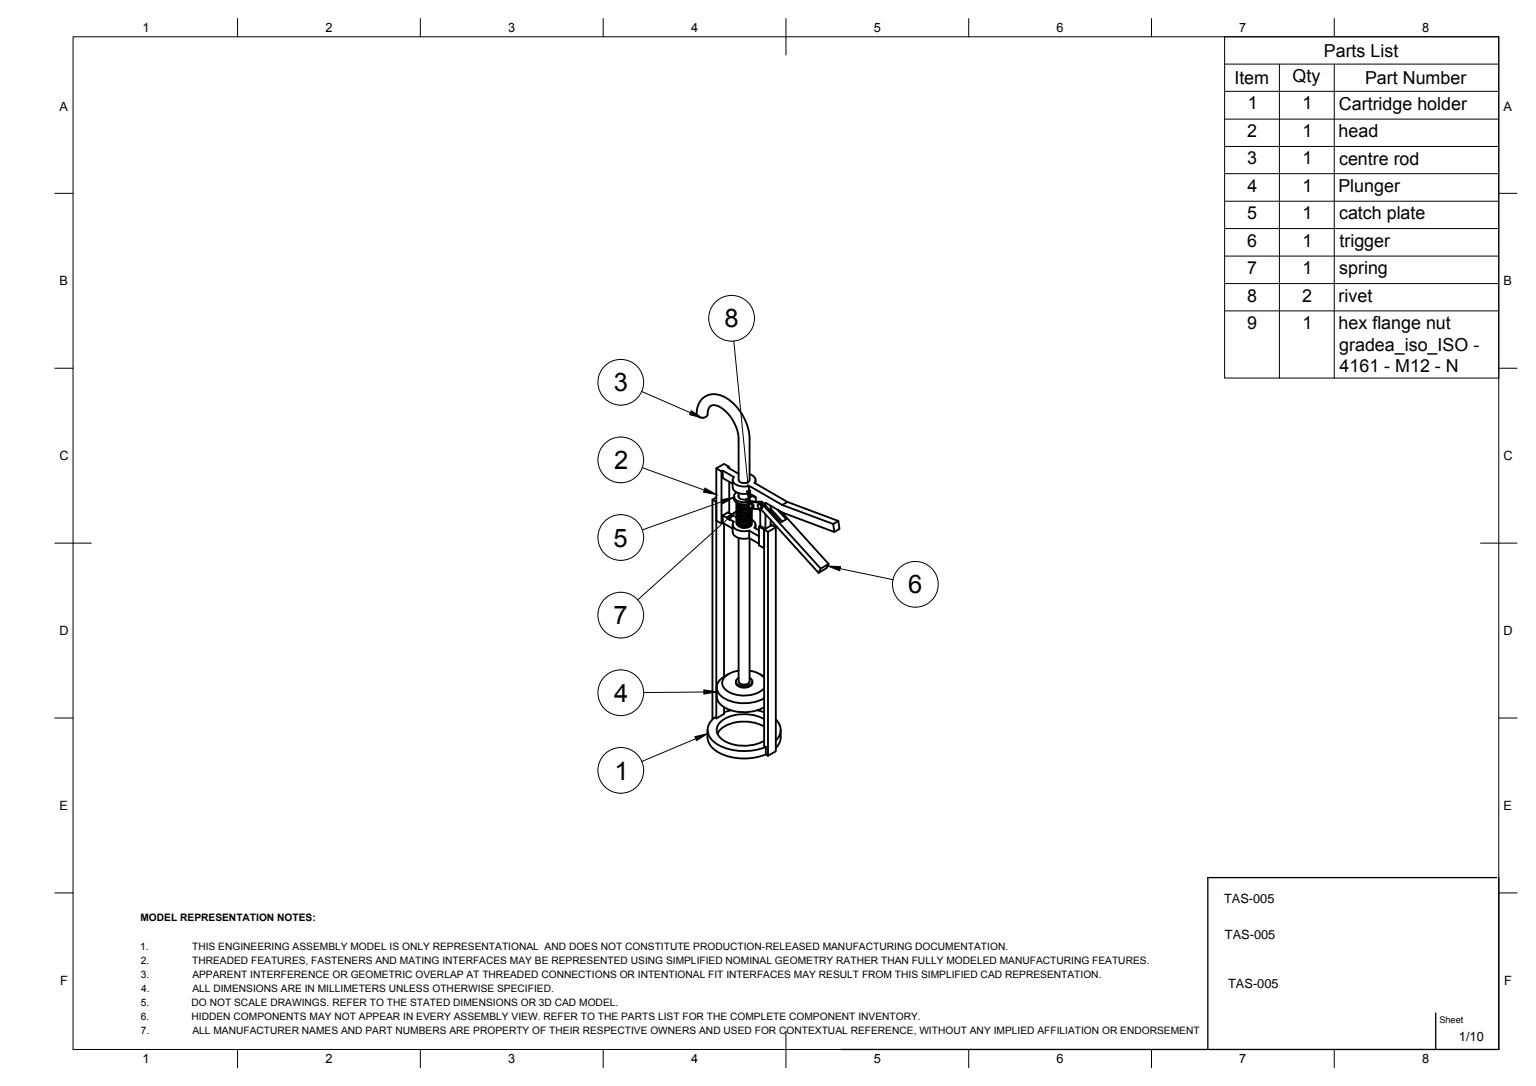
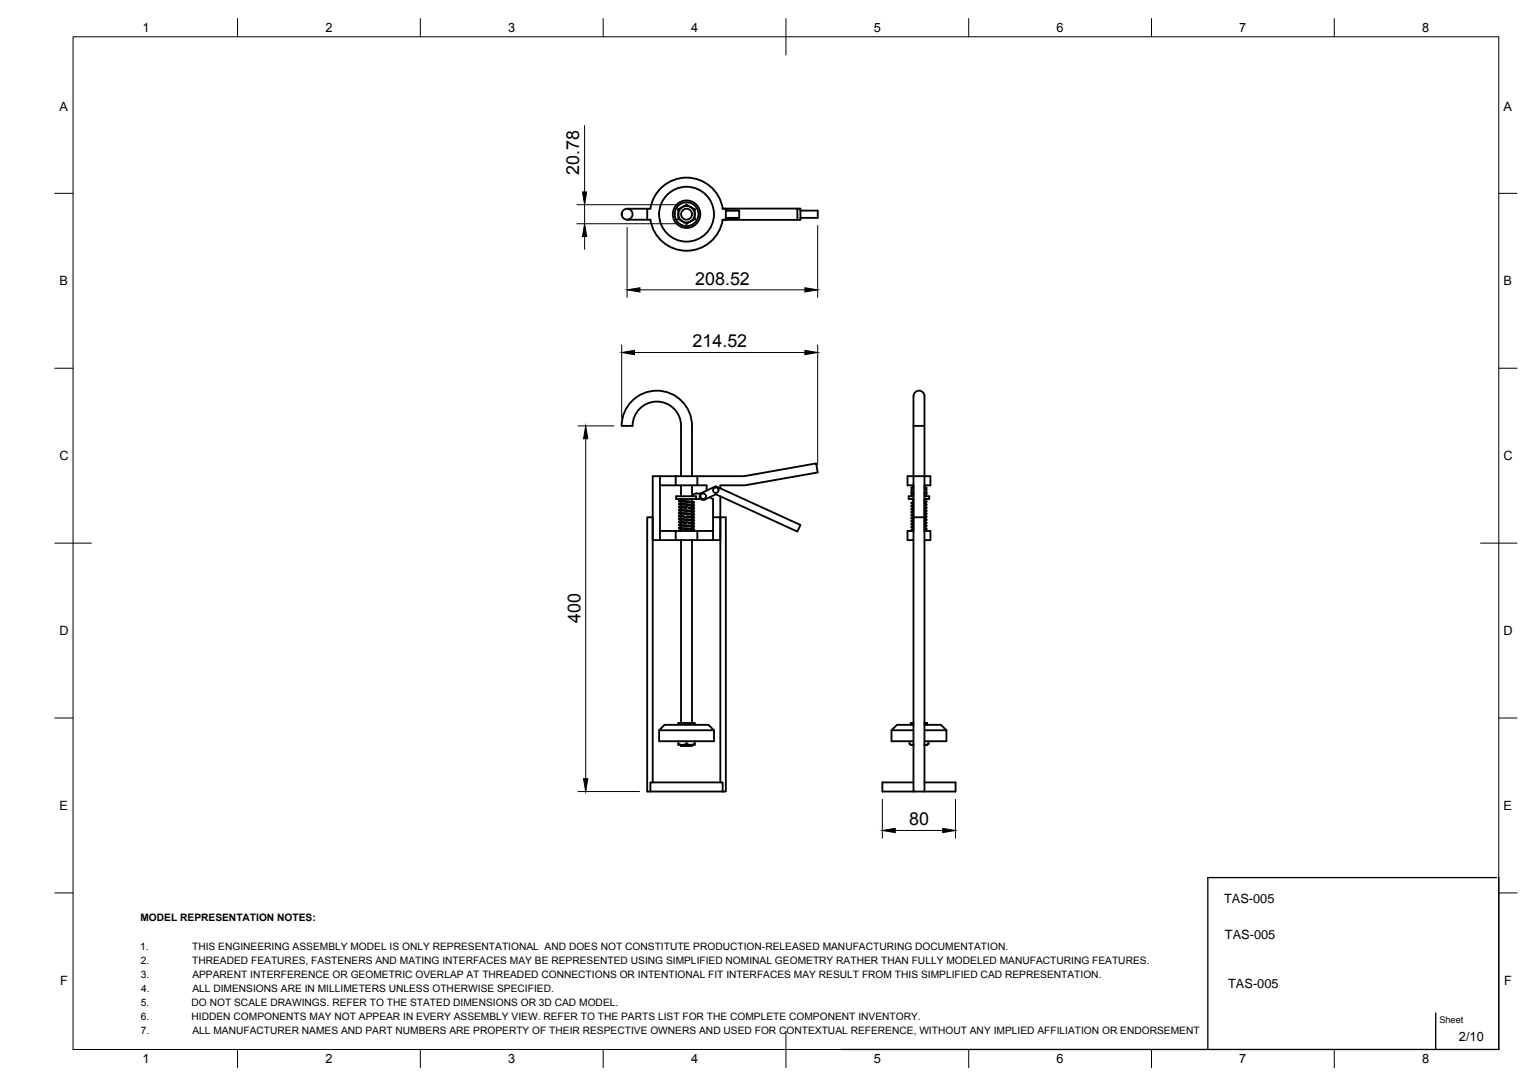
ISO-10303-21;
HEADER;
/* Generated by software containing ST-Developer
 * from STEP Tools, Inc. (www.steptools.com) 
 */

FILE_DESCRIPTION(
/* description */ ('STEP AP214'),
/* implementation_level */ '2;1');

FILE_NAME(
/* name */ 'TAS-005',
/* time_stamp */ '2026-11-04T19:54:22-08:00',
/* author */ (''),
/* organization */ (''),
/* preprocessor_version */ 'ST-DEVELOPER v20.2',
/* originating_system */ 'Autodesk Translation Framework v15.17.0.0',
/* authorisation */ '');

FILE_SCHEMA (('AUTOMOTIVE_DESIGN { 1 0 10303 214 3 1 1 }'));
ENDSEC;

DATA;
#10=MECHANICAL_DESIGN_GEOMETRIC_PRESENTATION_REPRESENTATION('',(#239,#240,
#241,#242,#243,#244,#245,#246,#247),#14084);
#11=ITEM_DEFINED_TRANSFORMATION($,$,#3575,#3854);
#12=ITEM_DEFINED_TRANSFORMATION($,$,#3597,#3855);
#13=ITEM_DEFINED_TRANSFORMATION($,$,#3649,#3856);
#14=ITEM_DEFINED_TRANSFORMATION($,$,#3725,#3857);
#15=ITEM_DEFINED_TRANSFORMATION($,$,#3741,#3858);
#16=ITEM_DEFINED_TRANSFORMATION($,$,#3763,#3859);
#17=ITEM_DEFINED_TRANSFORMATION($,$,#3794,#3860);
#18=ITEM_DEFINED_TRANSFORMATION($,$,#3840,#3861);
#19=ITEM_DEFINED_TRANSFORMATION($,$,#3802,#3862);
#20=ITEM_DEFINED_TRANSFORMATION($,$,#3840,#3863);
#21=(
REPRESENTATION_RELATIONSHIP($,$,#14120,#14119)
REPRESENTATION_RELATIONSHIP_WITH_TRANSFORMATION(#11)
SHAPE_REPRESENTATION_RELATIONSHIP()
);
#22=(
REPRESENTATION_RELATIONSHIP($,$,#14121,#14119)
REPRESENTATION_RELATIONSHIP_WITH_TRANSFORMATION(#12)
SHAPE_REPRESENTATION_RELATIONSHIP()
);
#23=(
REPRESENTATION_RELATIONSHIP($,$,#14122,#14119)
REPRESENTATION_RELATIONSHIP_WITH_TRANSFORMATION(#13)
SHAPE_REPRESENTATION_RELATIONSHIP()
);
#24=(
REPRESENTATION_RELATIONSHIP($,$,#14123,#14119)
REPRESENTATION_RELATIONSHIP_WITH_TRANSFORMATION(#14)
SHAPE_REPRESENTATION_RELATIONSHIP()
);
#25=(
REPRESENTATION_RELATIONSHIP($,$,#14124,#14119)
REPRESENTATION_RELATIONSHIP_WITH_TRANSFORMATION(#15)
SHAPE_REPRESENTATION_RELATIONSHIP()
);
#26=(
REPRESENTATION_RELATIONSHIP($,$,#14125,#14119)
REPRESENTATION_RELATIONSHIP_WITH_TRANSFORMATION(#16)
SHAPE_REPRESENTATION_RELATIONSHIP()
);
#27=(
REPRESENTATION_RELATIONSHIP($,$,#14126,#14119)
REPRESENTATION_RELATIONSHIP_WITH_TRANSFORMATION(#17)
SHAPE_REPRESENTATION_RELATIONSHIP()
);
#28=(
REPRESENTATION_RELATIONSHIP($,$,#14128,#14119)
REPRESENTATION_RELATIONSHIP_WITH_TRANSFORMATION(#18)
SHAPE_REPRESENTATION_RELATIONSHIP()
);
#29=(
REPRESENTATION_RELATIONSHIP($,$,#14127,#14119)
REPRESENTATION_RELATIONSHIP_WITH_TRANSFORMATION(#19)
SHAPE_REPRESENTATION_RELATIONSHIP()
);
#30=(
REPRESENTATION_RELATIONSHIP($,$,#14128,#14119)
REPRESENTATION_RELATIONSHIP_WITH_TRANSFORMATION(#20)
SHAPE_REPRESENTATION_RELATIONSHIP()
);
#31=CONTEXT_DEPENDENT_SHAPE_REPRESENTATION(#21,#14109);
#32=CONTEXT_DEPENDENT_SHAPE_REPRESENTATION(#22,#14110);
#33=CONTEXT_DEPENDENT_SHAPE_REPRESENTATION(#23,#14111);
#34=CONTEXT_DEPENDENT_SHAPE_REPRESENTATION(#24,#14112);
#35=CONTEXT_DEPENDENT_SHAPE_REPRESENTATION(#25,#14113);
#36=CONTEXT_DEPENDENT_SHAPE_REPRESENTATION(#26,#14114);
#37=CONTEXT_DEPENDENT_SHAPE_REPRESENTATION(#27,#14115);
#38=CONTEXT_DEPENDENT_SHAPE_REPRESENTATION(#28,#14116);
#39=CONTEXT_DEPENDENT_SHAPE_REPRESENTATION(#29,#14117);
#40=CONTEXT_DEPENDENT_SHAPE_REPRESENTATION(#30,#14118);
#41=NEXT_ASSEMBLY_USAGE_OCCURRENCE('Cartridge holder:1',
'Cartridge holder:1','Cartridge holder:1',#14130,#14131,
'Cartridge holder:1');
#42=NEXT_ASSEMBLY_USAGE_OCCURRENCE('head:1','head:1','head:1',#14130,#14132,
'head:1');
#43=NEXT_ASSEMBLY_USAGE_OCCURRENCE('centre rod:1','centre rod:1',
'centre rod:1',#14130,#14133,'centre rod:1');
#44=NEXT_ASSEMBLY_USAGE_OCCURRENCE('plunger:1','plunger:1','plunger:1',
#14130,#14134,'plunger:1');
#45=NEXT_ASSEMBLY_USAGE_OCCURRENCE('catch plate:1','catch plate:1',
'catch plate:1',#14130,#14135,'catch plate:1');
#46=NEXT_ASSEMBLY_USAGE_OCCURRENCE('trigger:1','trigger:1','trigger:1',
#14130,#14136,'trigger:1');
#47=NEXT_ASSEMBLY_USAGE_OCCURRENCE('spring:1','spring:1','spring:1',#14130,
#14137,'spring:1');
#48=NEXT_ASSEMBLY_USAGE_OCCURRENCE('rivet:1','rivet:1','rivet:1',#14130,
#14139,'rivet:1');
#49=NEXT_ASSEMBLY_USAGE_OCCURRENCE(
'hex flange nut gradea_iso_ISO - 4161 - M12 - N:1',
'hex flange nut gradea_iso_ISO - 4161 - M12 - N:1',
'hex flange nut gradea_iso_ISO - 4161 - M12 - N:1',#14130,#14138,
'hex flange nut gradea_iso_ISO - 4161 - M12 - N:1');
#50=NEXT_ASSEMBLY_USAGE_OCCURRENCE('rivet:2','rivet:2','rivet:2',#14130,
#14139,'rivet:2');
#51=CONICAL_SURFACE('',#3729,30.,0.78539816339745);
#52=CONICAL_SURFACE('',#3807,6.,0.959931088596879);
#53=CONICAL_SURFACE('',#3810,5.01,0.959931088596881);
#54=CONICAL_SURFACE('',#3813,12.389406481562,1.22173047639605);
#55=CONICAL_SURFACE('',#3834,9.,0.85944549144248);
#56=CONICAL_SURFACE('',#3835,9.,0.85944549144248);
#57=CONICAL_SURFACE('',#3836,9.,0.85944549144248);
#58=CONICAL_SURFACE('',#3837,9.,0.85944549144248);
#59=CONICAL_SURFACE('',#3838,9.,0.85944549144248);
#60=CONICAL_SURFACE('',#3839,9.,0.85944549144248);
#61=(
BOUNDED_SURFACE()
B_SPLINE_SURFACE(1,2,((#7888,#7889,#7890,#7891,#7892,#7893,#7894,#7895,
#7896,#7897,#7898,#7899,#7900,#7901,#7902,#7903,#7904,#7905,#7906,#7907,
#7908,#7909,#7910,#7911,#7912,#7913,#7914,#7915,#7916,#7917,#7918,#7919,
#7920,#7921,#7922,#7923,#7924,#7925,#7926,#7927,#7928,#7929,#7930,#7931,
#7932,#7933,#7934,#7935,#7936,#7937,#7938,#7939,#7940,#7941,#7942,#7943,
#7944,#7945,#7946,#7947,#7948,#7949,#7950,#7951,#7952,#7953,#7954,#7955,
#7956,#7957,#7958,#7959,#7960,#7961,#7962,#7963,#7964,#7965,#7966,#7967,
#7968,#7969,#7970,#7971,#7972,#7973,#7974,#7975,#7976,#7977,#7978,#7979,
#7980,#7981,#7982,#7983,#7984,#7985,#7986,#7987,#7988,#7989,#7990,#7991,
#7992,#7993,#7994,#7995,#7996,#7997,#7998,#7999,#8000,#8001,#8002,#8003,
#8004,#8005,#8006,#8007,#8008,#8009,#8010,#8011,#8012,#8013,#8014,#8015,
#8016,#8017,#8018,#8019,#8020,#8021,#8022,#8023,#8024,#8025,#8026,#8027,
#8028,#8029,#8030,#8031,#8032,#8033,#8034,#8035,#8036,#8037,#8038,#8039,
#8040,#8041,#8042,#8043,#8044,#8045,#8046,#8047,#8048,#8049,#8050,#8051,
#8052,#8053,#8054,#8055,#8056,#8057,#8058,#8059,#8060,#8061,#8062,#8063,
#8064,#8065,#8066,#8067,#8068,#8069,#8070,#8071,#8072,#8073,#8074,#8075,
#8076,#8077,#8078,#8079,#8080,#8081,#8082,#8083,#8084,#8085,#8086,#8087,
#8088,#8089,#8090,#8091,#8092,#8093,#8094,#8095,#8096,#8097,#8098,#8099,
#8100,#8101,#8102,#8103,#8104,#8105,#8106,#8107,#8108,#8109,#8110,#8111,
#8112,#8113,#8114,#8115,#8116,#8117,#8118,#8119,#8120,#8121,#8122,#8123,
#8124,#8125,#8126,#8127,#8128,#8129,#8130,#8131,#8132,#8133,#8134,#8135,
#8136,#8137,#8138,#8139,#8140,#8141,#8142,#8143,#8144,#8145,#8146,#8147,
#8148,#8149,#8150,#8151,#8152,#8153,#8154,#8155,#8156,#8157,#8158,#8159,
#8160,#8161,#8162,#8163,#8164,#8165,#8166,#8167,#8168,#8169,#8170,#8171,
#8172,#8173,#8174,#8175,#8176,#8177,#8178,#8179,#8180,#8181,#8182,#8183,
#8184,#8185,#8186,#8187,#8188,#8189,#8190,#8191,#8192,#8193,#8194,#8195,
#8196,#8197,#8198,#8199,#8200,#8201,#8202,#8203,#8204,#8205,#8206,#8207,
#8208),(#8209,#8210,#8211,#8212,#8213,#8214,#8215,#8216,#8217,#8218,#8219,
#8220,#8221,#8222,#8223,#8224,#8225,#8226,#8227,#8228,#8229,#8230,#8231,
#8232,#8233,#8234,#8235,#8236,#8237,#8238,#8239,#8240,#8241,#8242,#8243,
#8244,#8245,#8246,#8247,#8248,#8249,#8250,#8251,#8252,#8253,#8254,#8255,
#8256,#8257,#8258,#8259,#8260,#8261,#8262,#8263,#8264,#8265,#8266,#8267,
#8268,#8269,#8270,#8271,#8272,#8273,#8274,#8275,#8276,#8277,#8278,#8279,
#8280,#8281,#8282,#8283,#8284,#8285,#8286,#8287,#8288,#8289,#8290,#8291,
#8292,#8293,#8294,#8295,#8296,#8297,#8298,#8299,#8300,#8301,#8302,#8303,
#8304,#8305,#8306,#8307,#8308,#8309,#8310,#8311,#8312,#8313,#8314,#8315,
#8316,#8317,#8318,#8319,#8320,#8321,#8322,#8323,#8324,#8325,#8326,#8327,
#8328,#8329,#8330,#8331,#8332,#8333,#8334,#8335,#8336,#8337,#8338,#8339,
#8340,#8341,#8342,#8343,#8344,#8345,#8346,#8347,#8348,#8349,#8350,#8351,
#8352,#8353,#8354,#8355,#8356,#8357,#8358,#8359,#8360,#8361,#8362,#8363,
#8364,#8365,#8366,#8367,#8368,#8369,#8370,#8371,#8372,#8373,#8374,#8375,
#8376,#8377,#8378,#8379,#8380,#8381,#8382,#8383,#8384,#8385,#8386,#8387,
#8388,#8389,#8390,#8391,#8392,#8393,#8394,#8395,#8396,#8397,#8398,#8399,
#8400,#8401,#8402,#8403,#8404,#8405,#8406,#8407,#8408,#8409,#8410,#8411,
#8412,#8413,#8414,#8415,#8416,#8417,#8418,#8419,#8420,#8421,#8422,#8423,
#8424,#8425,#8426,#8427,#8428,#8429,#8430,#8431,#8432,#8433,#8434,#8435,
#8436,#8437,#8438,#8439,#8440,#8441,#8442,#8443,#8444,#8445,#8446,#8447,
#8448,#8449,#8450,#8451,#8452,#8453,#8454,#8455,#8456,#8457,#8458,#8459,
#8460,#8461,#8462,#8463,#8464,#8465,#8466,#8467,#8468,#8469,#8470,#8471,
#8472,#8473,#8474,#8475,#8476,#8477,#8478,#8479,#8480,#8481,#8482,#8483,
#8484,#8485,#8486,#8487,#8488,#8489,#8490,#8491,#8492,#8493,#8494,#8495,
#8496,#8497,#8498,#8499,#8500,#8501,#8502,#8503,#8504,#8505,#8506,#8507,
#8508,#8509,#8510,#8511,#8512,#8513,#8514,#8515,#8516,#8517,#8518,#8519,
#8520,#8521,#8522,#8523,#8524,#8525,#8526,#8527,#8528,#8529)),
 .UNSPECIFIED.,.F.,.F.,.F.)
B_SPLINE_SURFACE_WITH_KNOTS((2,2),(3,2,2,2,2,2,2,2,2,2,2,2,2,2,2,2,2,2,
2,2,2,2,2,2,2,2,2,2,2,2,2,2,2,2,2,2,2,2,2,2,2,2,2,2,2,2,2,2,2,2,2,2,2,2,
2,2,2,2,2,2,2,2,2,2,2,2,2,2,2,2,2,2,2,2,2,2,2,2,2,2,2,2,2,2,2,2,2,2,2,2,
2,2,2,2,2,2,2,2,2,2,2,2,2,2,2,2,2,2,2,2,2,2,2,2,2,2,2,2,2,2,2,2,2,2,2,2,
2,2,2,2,2,2,2,2,2,2,2,2,2,2,2,2,2,2,2,2,2,2,2,2,2,2,2,2,2,2,2,2,2,2,3),
(0.,1.),(0.,0.00617283950617284,0.0123456790123457,0.0185185185185185,0.0246913580246914,
0.0308641975308642,0.037037037037037,0.0432098765432099,0.0493827160493827,
0.0555555555555556,0.0617283950617284,0.0679012345679012,0.0740740740740741,
0.0802469135802469,0.0864197530864197,0.0925925925925926,0.0987654320987654,
0.104938271604938,0.111111111111111,0.117283950617284,0.123456790123457,
0.12962962962963,0.135802469135802,0.141975308641975,0.148148148148148,
0.154320987654321,0.160493827160494,0.166666666666667,0.172839506172839,
0.179012345679012,0.185185185185185,0.191358024691358,0.197530864197531,
0.203703703703704,0.209876543209877,0.216049382716049,0.222222222222222,
0.228395061728395,0.234567901234568,0.240740740740741,0.246913580246914,
0.253086419753086,0.259259259259259,0.265432098765432,0.271604938271605,
0.277777777777778,0.283950617283951,0.290123456790123,0.296296296296296,
0.302469135802469,0.308641975308642,0.314814814814815,0.320987654320988,
0.327160493827161,0.333333333333333,0.339506172839506,0.345679012345679,
0.351851851851852,0.358024691358025,0.364197530864198,0.37037037037037,
0.376543209876543,0.382716049382716,0.388888888888889,0.395061728395062,
0.401234567901235,0.407407407407407,0.41358024691358,0.419753086419753,
0.425925925925926,0.432098765432099,0.438271604938272,0.444444444444444,
0.450617283950617,0.45679012345679,0.462962962962963,0.469135802469136,
0.475308641975309,0.481481481481481,0.487654320987654,0.493827160493827,
0.5,0.506172839506173,0.512345679012346,0.518518518518518,0.524691358024691,
0.530864197530864,0.537037037037037,0.54320987654321,0.549382716049383,
0.555555555555556,0.561728395061728,0.567901234567901,0.574074074074074,
0.580246913580247,0.58641975308642,0.592592592592593,0.598765432098765,
0.604938271604938,0.611111111111111,0.617283950617284,0.623456790123457,
0.62962962962963,0.635802469135803,0.641975308641975,0.648148148148148,
0.654320987654321,0.660493827160494,0.666666666666667,0.672839506172839,
0.679012345679012,0.685185185185185,0.691358024691358,0.697530864197531,
0.703703703703704,0.709876543209877,0.716049382716049,0.722222222222222,
0.728395061728395,0.734567901234568,0.740740740740741,0.746913580246914,
0.753086419753086,0.759259259259259,0.765432098765432,0.771604938271605,
0.777777777777778,0.783950617283951,0.790123456790123,0.796296296296296,
0.802469135802469,0.808641975308642,0.814814814814815,0.820987654320988,
0.827160493827161,0.833333333333333,0.839506172839506,0.845679012345679,
0.851851851851852,0.858024691358025,0.864197530864197,0.87037037037037,
0.876543209876543,0.882716049382716,0.888888888888889,0.895061728395062,
0.901234567901235,0.907407407407407,0.91358024691358,0.919753086419753,
0.925925925925926,0.932098765432099,0.938271604938272,0.944444444444444,
0.950617283950617,0.95679012345679,0.962962962962963,0.969135802469136,
0.975308641975309,0.981481481481482,0.987654320987654),.UNSPECIFIED.)
GEOMETRIC_REPRESENTATION_ITEM()
RATIONAL_B_SPLINE_SURFACE(((1.,0.866025403784439,1.,0.866025403784439,1.,
0.866025403784439,1.,0.866025403784439,1.,0.866025403784439,1.,0.866025403784439,
1.,0.866025403784439,1.,0.866025403784439,1.,0.866025403784439,1.,0.866025403784439,
1.,0.866025403784439,1.,0.866025403784439,1.,0.866025403784439,1.,0.866025403784439,
1.,0.866025403784439,1.,0.866025403784439,1.,0.866025403784439,1.,0.866025403784439,
1.,0.866025403784439,1.,0.866025403784439,1.,0.866025403784439,1.,0.866025403784439,
1.,0.866025403784439,1.,0.866025403784439,1.,0.866025403784439,1.,0.866025403784439,
1.,0.866025403784439,1.,0.866025403784439,1.,0.866025403784439,1.,0.866025403784439,
1.,0.866025403784439,1.,0.866025403784439,1.,0.866025403784439,1.,0.866025403784439,
1.,0.866025403784439,1.,0.866025403784439,1.,0.866025403784439,1.,0.866025403784439,
1.,0.866025403784439,1.,0.866025403784439,1.,0.866025403784439,1.,0.866025403784439,
1.,0.866025403784439,1.,0.866025403784439,1.,0.866025403784439,1.,0.866025403784439,
1.,0.866025403784439,1.,0.866025403784439,1.,0.866025403784439,1.,0.866025403784439,
1.,0.866025403784439,1.,0.866025403784439,1.,0.866025403784439,1.,0.866025403784439,
1.,0.866025403784439,1.,0.866025403784439,1.,0.866025403784439,1.,0.866025403784439,
1.,0.866025403784439,1.,0.866025403784439,1.,0.866025403784439,1.,0.866025403784439,
1.,0.866025403784439,1.,0.866025403784439,1.,0.866025403784439,1.,0.866025403784439,
1.,0.866025403784439,1.,0.866025403784439,1.,0.866025403784439,1.,0.866025403784439,
1.,0.866025403784439,1.,0.866025403784439,1.,0.866025403784439,1.,0.866025403784439,
1.,0.866025403784439,1.,0.866025403784439,1.,0.866025403784439,1.,0.866025403784439,
1.,0.866025403784439,1.,0.866025403784439,1.,0.866025403784439,1.,0.866025403784439,
1.,0.866025403784439,1.,0.866025403784439,1.,0.866025403784439,1.,0.866025403784439,
1.,0.866025403784439,1.,0.866025403784439,1.,0.866025403784439,1.,0.866025403784439,
1.,0.866025403784439,1.,0.866025403784439,1.,0.866025403784439,1.,0.866025403784439,
1.,0.866025403784439,1.,0.866025403784439,1.,0.866025403784439,1.,0.866025403784439,
1.,0.866025403784439,1.,0.866025403784439,1.,0.866025403784439,1.,0.866025403784439,
1.,0.866025403784439,1.,0.866025403784439,1.,0.866025403784439,1.,0.866025403784439,
1.,0.866025403784439,1.,0.866025403784439,1.,0.866025403784439,1.,0.866025403784439,
1.,0.866025403784439,1.,0.866025403784439,1.,0.866025403784439,1.,0.866025403784439,
1.,0.866025403784439,1.,0.866025403784439,1.,0.866025403784439,1.,0.866025403784439,
1.,0.866025403784439,1.,0.866025403784439,1.,0.866025403784439,1.,0.866025403784439,
1.,0.866025403784439,1.,0.866025403784439,1.,0.866025403784439,1.,0.866025403784439,
1.,0.866025403784439,1.,0.866025403784439,1.,0.866025403784439,1.,0.866025403784439,
1.,0.866025403784439,1.,0.866025403784439,1.,0.866025403784439,1.,0.866025403784439,
1.,0.866025403784439,1.,0.866025403784439,1.,0.866025403784439,1.,0.866025403784439,
1.,0.866025403784439,1.,0.866025403784439,1.,0.866025403784439,1.,0.866025403784439,
1.,0.866025403784439,1.,0.866025403784439,1.,0.866025403784439,1.,0.866025403784439,
1.,0.866025403784439,1.,0.866025403784439,1.,0.866025403784439,1.,0.866025403784439,
1.,0.866025403784439,1.,0.866025403784439,1.,0.866025403784439,1.,0.866025403784439,
1.,0.866025403784439,1.,0.866025403784439,1.,0.866025403784439,1.,0.866025403784439,
1.,0.866025403784439,1.,0.866025403784439,1.),(1.,0.866025403784439,1.,
0.866025403784439,1.,0.866025403784439,1.,0.866025403784439,1.,0.866025403784439,
1.,0.866025403784439,1.,0.866025403784439,1.,0.866025403784439,1.,0.866025403784439,
1.,0.866025403784439,1.,0.866025403784439,1.,0.866025403784439,1.,0.866025403784439,
1.,0.866025403784439,1.,0.866025403784439,1.,0.866025403784439,1.,0.866025403784439,
1.,0.866025403784439,1.,0.866025403784439,1.,0.866025403784439,1.,0.866025403784439,
1.,0.866025403784439,1.,0.866025403784439,1.,0.866025403784439,1.,0.866025403784439,
1.,0.866025403784439,1.,0.866025403784439,1.,0.866025403784439,1.,0.866025403784439,
1.,0.866025403784439,1.,0.866025403784439,1.,0.866025403784439,1.,0.866025403784439,
1.,0.866025403784439,1.,0.866025403784439,1.,0.866025403784439,1.,0.866025403784439,
1.,0.866025403784439,1.,0.866025403784439,1.,0.866025403784439,1.,0.866025403784439,
1.,0.866025403784439,1.,0.866025403784439,1.,0.866025403784439,1.,0.866025403784439,
1.,0.866025403784439,1.,0.866025403784439,1.,0.866025403784439,1.,0.866025403784439,
1.,0.866025403784439,1.,0.866025403784439,1.,0.866025403784439,1.,0.866025403784439,
1.,0.866025403784439,1.,0.866025403784439,1.,0.866025403784439,1.,0.866025403784439,
1.,0.866025403784439,1.,0.866025403784439,1.,0.866025403784439,1.,0.866025403784439,
1.,0.866025403784439,1.,0.866025403784439,1.,0.866025403784439,1.,0.866025403784439,
1.,0.866025403784439,1.,0.866025403784439,1.,0.866025403784439,1.,0.866025403784439,
1.,0.866025403784439,1.,0.866025403784439,1.,0.866025403784439,1.,0.866025403784439,
1.,0.866025403784439,1.,0.866025403784439,1.,0.866025403784439,1.,0.866025403784439,
1.,0.866025403784439,1.,0.866025403784439,1.,0.866025403784439,1.,0.866025403784439,
1.,0.866025403784439,1.,0.866025403784439,1.,0.866025403784439,1.,0.866025403784439,
1.,0.866025403784439,1.,0.866025403784439,1.,0.866025403784439,1.,0.866025403784439,
1.,0.866025403784439,1.,0.866025403784439,1.,0.866025403784439,1.,0.866025403784439,
1.,0.866025403784439,1.,0.866025403784439,1.,0.866025403784439,1.,0.866025403784439,
1.,0.866025403784439,1.,0.866025403784439,1.,0.866025403784439,1.,0.866025403784439,
1.,0.866025403784439,1.,0.866025403784439,1.,0.866025403784439,1.,0.866025403784439,
1.,0.866025403784439,1.,0.866025403784439,1.,0.866025403784439,1.,0.866025403784439,
1.,0.866025403784439,1.,0.866025403784439,1.,0.866025403784439,1.,0.866025403784439,
1.,0.866025403784439,1.,0.866025403784439,1.,0.866025403784439,1.,0.866025403784439,
1.,0.866025403784439,1.,0.866025403784439,1.,0.866025403784439,1.,0.866025403784439,
1.,0.866025403784439,1.,0.866025403784439,1.,0.866025403784439,1.,0.866025403784439,
1.,0.866025403784439,1.,0.866025403784439,1.,0.866025403784439,1.,0.866025403784439,
1.,0.866025403784439,1.,0.866025403784439,1.,0.866025403784439,1.,0.866025403784439,
1.,0.866025403784439,1.,0.866025403784439,1.,0.866025403784439,1.,0.866025403784439,
1.,0.866025403784439,1.,0.866025403784439,1.,0.866025403784439,1.,0.866025403784439,
1.,0.866025403784439,1.,0.866025403784439,1.,0.866025403784439,1.,0.866025403784439,
1.,0.866025403784439,1.,0.866025403784439,1.,0.866025403784439,1.,0.866025403784439,
1.,0.866025403784439,1.,0.866025403784439,1.,0.866025403784439,1.,0.866025403784439,
1.,0.866025403784439,1.,0.866025403784439,1.,0.866025403784439,1.,0.866025403784439,
1.,0.866025403784439,1.,0.866025403784439,1.,0.866025403784439,1.)))
REPRESENTATION_ITEM('')
SURFACE()
);
#62=(
BOUNDED_SURFACE()
B_SPLINE_SURFACE(1,2,((#8545,#8546,#8547,#8548,#8549,#8550,#8551,#8552,
#8553,#8554,#8555,#8556,#8557,#8558,#8559,#8560,#8561,#8562,#8563,#8564,
#8565,#8566,#8567,#8568,#8569,#8570,#8571,#8572,#8573,#8574,#8575,#8576,
#8577,#8578,#8579,#8580,#8581,#8582,#8583,#8584,#8585,#8586,#8587,#8588,
#8589,#8590,#8591,#8592,#8593,#8594,#8595,#8596,#8597,#8598,#8599,#8600,
#8601,#8602,#8603,#8604,#8605,#8606,#8607,#8608,#8609,#8610,#8611,#8612,
#8613,#8614,#8615,#8616,#8617,#8618,#8619,#8620,#8621,#8622,#8623,#8624,
#8625,#8626,#8627,#8628,#8629,#8630,#8631,#8632,#8633,#8634,#8635,#8636,
#8637,#8638,#8639,#8640,#8641,#8642,#8643,#8644,#8645,#8646,#8647,#8648,
#8649,#8650,#8651,#8652,#8653,#8654,#8655,#8656,#8657,#8658,#8659,#8660,
#8661,#8662,#8663,#8664,#8665,#8666,#8667,#8668,#8669,#8670,#8671,#8672,
#8673,#8674,#8675,#8676,#8677,#8678,#8679,#8680,#8681,#8682,#8683,#8684,
#8685,#8686,#8687,#8688,#8689,#8690,#8691,#8692,#8693,#8694,#8695,#8696,
#8697,#8698,#8699,#8700,#8701,#8702,#8703,#8704,#8705,#8706,#8707,#8708,
#8709,#8710,#8711,#8712,#8713,#8714,#8715,#8716,#8717,#8718,#8719,#8720,
#8721,#8722,#8723,#8724,#8725,#8726,#8727,#8728,#8729,#8730,#8731,#8732,
#8733,#8734,#8735,#8736,#8737,#8738,#8739,#8740,#8741,#8742,#8743,#8744,
#8745,#8746,#8747,#8748,#8749,#8750,#8751,#8752,#8753,#8754,#8755,#8756,
#8757,#8758,#8759,#8760,#8761,#8762,#8763,#8764,#8765,#8766,#8767,#8768,
#8769,#8770,#8771,#8772,#8773,#8774,#8775,#8776,#8777,#8778,#8779,#8780,
#8781,#8782,#8783,#8784,#8785,#8786,#8787,#8788,#8789,#8790,#8791,#8792,
#8793,#8794,#8795,#8796,#8797,#8798,#8799,#8800,#8801,#8802,#8803,#8804,
#8805,#8806,#8807,#8808,#8809,#8810,#8811,#8812,#8813,#8814,#8815,#8816,
#8817,#8818,#8819,#8820,#8821,#8822,#8823,#8824,#8825,#8826,#8827,#8828,
#8829,#8830,#8831,#8832,#8833,#8834,#8835,#8836,#8837,#8838,#8839,#8840,
#8841,#8842,#8843,#8844,#8845,#8846,#8847,#8848,#8849,#8850,#8851,#8852,
#8853,#8854,#8855,#8856,#8857,#8858,#8859,#8860,#8861,#8862,#8863,#8864,
#8865),(#8866,#8867,#8868,#8869,#8870,#8871,#8872,#8873,#8874,#8875,#8876,
#8877,#8878,#8879,#8880,#8881,#8882,#8883,#8884,#8885,#8886,#8887,#8888,
#8889,#8890,#8891,#8892,#8893,#8894,#8895,#8896,#8897,#8898,#8899,#8900,
#8901,#8902,#8903,#8904,#8905,#8906,#8907,#8908,#8909,#8910,#8911,#8912,
#8913,#8914,#8915,#8916,#8917,#8918,#8919,#8920,#8921,#8922,#8923,#8924,
#8925,#8926,#8927,#8928,#8929,#8930,#8931,#8932,#8933,#8934,#8935,#8936,
#8937,#8938,#8939,#8940,#8941,#8942,#8943,#8944,#8945,#8946,#8947,#8948,
#8949,#8950,#8951,#8952,#8953,#8954,#8955,#8956,#8957,#8958,#8959,#8960,
#8961,#8962,#8963,#8964,#8965,#8966,#8967,#8968,#8969,#8970,#8971,#8972,
#8973,#8974,#8975,#8976,#8977,#8978,#8979,#8980,#8981,#8982,#8983,#8984,
#8985,#8986,#8987,#8988,#8989,#8990,#8991,#8992,#8993,#8994,#8995,#8996,
#8997,#8998,#8999,#9000,#9001,#9002,#9003,#9004,#9005,#9006,#9007,#9008,
#9009,#9010,#9011,#9012,#9013,#9014,#9015,#9016,#9017,#9018,#9019,#9020,
#9021,#9022,#9023,#9024,#9025,#9026,#9027,#9028,#9029,#9030,#9031,#9032,
#9033,#9034,#9035,#9036,#9037,#9038,#9039,#9040,#9041,#9042,#9043,#9044,
#9045,#9046,#9047,#9048,#9049,#9050,#9051,#9052,#9053,#9054,#9055,#9056,
#9057,#9058,#9059,#9060,#9061,#9062,#9063,#9064,#9065,#9066,#9067,#9068,
#9069,#9070,#9071,#9072,#9073,#9074,#9075,#9076,#9077,#9078,#9079,#9080,
#9081,#9082,#9083,#9084,#9085,#9086,#9087,#9088,#9089,#9090,#9091,#9092,
#9093,#9094,#9095,#9096,#9097,#9098,#9099,#9100,#9101,#9102,#9103,#9104,
#9105,#9106,#9107,#9108,#9109,#9110,#9111,#9112,#9113,#9114,#9115,#9116,
#9117,#9118,#9119,#9120,#9121,#9122,#9123,#9124,#9125,#9126,#9127,#9128,
#9129,#9130,#9131,#9132,#9133,#9134,#9135,#9136,#9137,#9138,#9139,#9140,
#9141,#9142,#9143,#9144,#9145,#9146,#9147,#9148,#9149,#9150,#9151,#9152,
#9153,#9154,#9155,#9156,#9157,#9158,#9159,#9160,#9161,#9162,#9163,#9164,
#9165,#9166,#9167,#9168,#9169,#9170,#9171,#9172,#9173,#9174,#9175,#9176,
#9177,#9178,#9179,#9180,#9181,#9182,#9183,#9184,#9185,#9186)),
 .UNSPECIFIED.,.F.,.F.,.F.)
B_SPLINE_SURFACE_WITH_KNOTS((2,2),(3,2,2,2,2,2,2,2,2,2,2,2,2,2,2,2,2,2,
2,2,2,2,2,2,2,2,2,2,2,2,2,2,2,2,2,2,2,2,2,2,2,2,2,2,2,2,2,2,2,2,2,2,2,2,
2,2,2,2,2,2,2,2,2,2,2,2,2,2,2,2,2,2,2,2,2,2,2,2,2,2,2,2,2,2,2,2,2,2,2,2,
2,2,2,2,2,2,2,2,2,2,2,2,2,2,2,2,2,2,2,2,2,2,2,2,2,2,2,2,2,2,2,2,2,2,2,2,
2,2,2,2,2,2,2,2,2,2,2,2,2,2,2,2,2,2,2,2,2,2,2,2,2,2,2,2,2,2,2,2,2,2,3),
(0.,1.),(0.,0.00617283950617284,0.0123456790123457,0.0185185185185185,0.0246913580246914,
0.0308641975308642,0.037037037037037,0.0432098765432099,0.0493827160493827,
0.0555555555555556,0.0617283950617284,0.0679012345679012,0.0740740740740741,
0.0802469135802469,0.0864197530864197,0.0925925925925926,0.0987654320987654,
0.104938271604938,0.111111111111111,0.117283950617284,0.123456790123457,
0.12962962962963,0.135802469135802,0.141975308641975,0.148148148148148,
0.154320987654321,0.160493827160494,0.166666666666667,0.172839506172839,
0.179012345679012,0.185185185185185,0.191358024691358,0.197530864197531,
0.203703703703704,0.209876543209877,0.216049382716049,0.222222222222222,
0.228395061728395,0.234567901234568,0.240740740740741,0.246913580246914,
0.253086419753086,0.259259259259259,0.265432098765432,0.271604938271605,
0.277777777777778,0.283950617283951,0.290123456790123,0.296296296296296,
0.302469135802469,0.308641975308642,0.314814814814815,0.320987654320988,
0.327160493827161,0.333333333333333,0.339506172839506,0.345679012345679,
0.351851851851852,0.358024691358025,0.364197530864198,0.37037037037037,
0.376543209876543,0.382716049382716,0.388888888888889,0.395061728395062,
0.401234567901235,0.407407407407407,0.41358024691358,0.419753086419753,
0.425925925925926,0.432098765432099,0.438271604938272,0.444444444444444,
0.450617283950617,0.45679012345679,0.462962962962963,0.469135802469136,
0.475308641975309,0.481481481481481,0.487654320987654,0.493827160493827,
0.5,0.506172839506173,0.512345679012346,0.518518518518518,0.524691358024691,
0.530864197530864,0.537037037037037,0.54320987654321,0.549382716049383,
0.555555555555556,0.561728395061728,0.567901234567901,0.574074074074074,
0.580246913580247,0.58641975308642,0.592592592592593,0.598765432098765,
0.604938271604938,0.611111111111111,0.617283950617284,0.623456790123457,
0.62962962962963,0.635802469135803,0.641975308641975,0.648148148148148,
0.654320987654321,0.660493827160494,0.666666666666667,0.672839506172839,
0.679012345679012,0.685185185185185,0.691358024691358,0.697530864197531,
0.703703703703704,0.709876543209877,0.716049382716049,0.722222222222222,
0.728395061728395,0.734567901234568,0.740740740740741,0.746913580246914,
0.753086419753086,0.759259259259259,0.765432098765432,0.771604938271605,
0.777777777777778,0.783950617283951,0.790123456790123,0.796296296296296,
0.802469135802469,0.808641975308642,0.814814814814815,0.820987654320988,
0.827160493827161,0.833333333333333,0.839506172839506,0.845679012345679,
0.851851851851852,0.858024691358025,0.864197530864197,0.87037037037037,
0.876543209876543,0.882716049382716,0.888888888888889,0.895061728395062,
0.901234567901235,0.907407407407407,0.91358024691358,0.919753086419753,
0.925925925925926,0.932098765432099,0.938271604938272,0.944444444444444,
0.950617283950617,0.95679012345679,0.962962962962963,0.969135802469136,
0.975308641975309,0.981481481481482,0.987654320987654),.UNSPECIFIED.)
GEOMETRIC_REPRESENTATION_ITEM()
RATIONAL_B_SPLINE_SURFACE(((1.,0.866025403784439,1.,0.866025403784439,1.,
0.866025403784439,1.,0.866025403784439,1.,0.866025403784439,1.,0.866025403784439,
1.,0.866025403784439,1.,0.866025403784439,1.,0.866025403784439,1.,0.866025403784439,
1.,0.866025403784439,1.,0.866025403784439,1.,0.866025403784439,1.,0.866025403784439,
1.,0.866025403784439,1.,0.866025403784439,1.,0.866025403784439,1.,0.866025403784439,
1.,0.866025403784439,1.,0.866025403784439,1.,0.866025403784439,1.,0.866025403784439,
1.,0.866025403784439,1.,0.866025403784439,1.,0.866025403784439,1.,0.866025403784439,
1.,0.866025403784439,1.,0.866025403784439,1.,0.866025403784439,1.,0.866025403784439,
1.,0.866025403784439,1.,0.866025403784439,1.,0.866025403784439,1.,0.866025403784439,
1.,0.866025403784439,1.,0.866025403784439,1.,0.866025403784439,1.,0.866025403784439,
1.,0.866025403784439,1.,0.866025403784439,1.,0.866025403784439,1.,0.866025403784439,
1.,0.866025403784439,1.,0.866025403784439,1.,0.866025403784439,1.,0.866025403784439,
1.,0.866025403784439,1.,0.866025403784439,1.,0.866025403784439,1.,0.866025403784439,
1.,0.866025403784439,1.,0.866025403784439,1.,0.866025403784439,1.,0.866025403784439,
1.,0.866025403784439,1.,0.866025403784439,1.,0.866025403784439,1.,0.866025403784439,
1.,0.866025403784439,1.,0.866025403784439,1.,0.866025403784439,1.,0.866025403784439,
1.,0.866025403784439,1.,0.866025403784439,1.,0.866025403784439,1.,0.866025403784439,
1.,0.866025403784439,1.,0.866025403784439,1.,0.866025403784439,1.,0.866025403784439,
1.,0.866025403784439,1.,0.866025403784439,1.,0.866025403784439,1.,0.866025403784439,
1.,0.866025403784439,1.,0.866025403784439,1.,0.866025403784439,1.,0.866025403784439,
1.,0.866025403784439,1.,0.866025403784439,1.,0.866025403784439,1.,0.866025403784439,
1.,0.866025403784439,1.,0.866025403784439,1.,0.866025403784439,1.,0.866025403784439,
1.,0.866025403784439,1.,0.866025403784439,1.,0.866025403784439,1.,0.866025403784439,
1.,0.866025403784439,1.,0.866025403784439,1.,0.866025403784439,1.,0.866025403784439,
1.,0.866025403784439,1.,0.866025403784439,1.,0.866025403784439,1.,0.866025403784439,
1.,0.866025403784439,1.,0.866025403784439,1.,0.866025403784439,1.,0.866025403784439,
1.,0.866025403784439,1.,0.866025403784439,1.,0.866025403784439,1.,0.866025403784439,
1.,0.866025403784439,1.,0.866025403784439,1.,0.866025403784439,1.,0.866025403784439,
1.,0.866025403784439,1.,0.866025403784439,1.,0.866025403784439,1.,0.866025403784439,
1.,0.866025403784439,1.,0.866025403784439,1.,0.866025403784439,1.,0.866025403784439,
1.,0.866025403784439,1.,0.866025403784439,1.,0.866025403784439,1.,0.866025403784439,
1.,0.866025403784439,1.,0.866025403784439,1.,0.866025403784439,1.,0.866025403784439,
1.,0.866025403784439,1.,0.866025403784439,1.,0.866025403784439,1.,0.866025403784439,
1.,0.866025403784439,1.,0.866025403784439,1.,0.866025403784439,1.,0.866025403784439,
1.,0.866025403784439,1.,0.866025403784439,1.,0.866025403784439,1.,0.866025403784439,
1.,0.866025403784439,1.,0.866025403784439,1.,0.866025403784439,1.,0.866025403784439,
1.,0.866025403784439,1.,0.866025403784439,1.,0.866025403784439,1.,0.866025403784439,
1.,0.866025403784439,1.,0.866025403784439,1.,0.866025403784439,1.,0.866025403784439,
1.,0.866025403784439,1.,0.866025403784439,1.,0.866025403784439,1.,0.866025403784439,
1.,0.866025403784439,1.,0.866025403784439,1.,0.866025403784439,1.,0.866025403784439,
1.,0.866025403784439,1.,0.866025403784439,1.),(1.,0.866025403784439,1.,
0.866025403784439,1.,0.866025403784439,1.,0.866025403784439,1.,0.866025403784439,
1.,0.866025403784439,1.,0.866025403784439,1.,0.866025403784439,1.,0.866025403784439,
1.,0.866025403784439,1.,0.866025403784439,1.,0.866025403784439,1.,0.866025403784439,
1.,0.866025403784439,1.,0.866025403784439,1.,0.866025403784439,1.,0.866025403784439,
1.,0.866025403784439,1.,0.866025403784439,1.,0.866025403784439,1.,0.866025403784439,
1.,0.866025403784439,1.,0.866025403784439,1.,0.866025403784439,1.,0.866025403784439,
1.,0.866025403784439,1.,0.866025403784439,1.,0.866025403784439,1.,0.866025403784439,
1.,0.866025403784439,1.,0.866025403784439,1.,0.866025403784439,1.,0.866025403784439,
1.,0.866025403784439,1.,0.866025403784439,1.,0.866025403784439,1.,0.866025403784439,
1.,0.866025403784439,1.,0.866025403784439,1.,0.866025403784439,1.,0.866025403784439,
1.,0.866025403784439,1.,0.866025403784439,1.,0.866025403784439,1.,0.866025403784439,
1.,0.866025403784439,1.,0.866025403784439,1.,0.866025403784439,1.,0.866025403784439,
1.,0.866025403784439,1.,0.866025403784439,1.,0.866025403784439,1.,0.866025403784439,
1.,0.866025403784439,1.,0.866025403784439,1.,0.866025403784439,1.,0.866025403784439,
1.,0.866025403784439,1.,0.866025403784439,1.,0.866025403784439,1.,0.866025403784439,
1.,0.866025403784439,1.,0.866025403784439,1.,0.866025403784439,1.,0.866025403784439,
1.,0.866025403784439,1.,0.866025403784439,1.,0.866025403784439,1.,0.866025403784439,
1.,0.866025403784439,1.,0.866025403784439,1.,0.866025403784439,1.,0.866025403784439,
1.,0.866025403784439,1.,0.866025403784439,1.,0.866025403784439,1.,0.866025403784439,
1.,0.866025403784439,1.,0.866025403784439,1.,0.866025403784439,1.,0.866025403784439,
1.,0.866025403784439,1.,0.866025403784439,1.,0.866025403784439,1.,0.866025403784439,
1.,0.866025403784439,1.,0.866025403784439,1.,0.866025403784439,1.,0.866025403784439,
1.,0.866025403784439,1.,0.866025403784439,1.,0.866025403784439,1.,0.866025403784439,
1.,0.866025403784439,1.,0.866025403784439,1.,0.866025403784439,1.,0.866025403784439,
1.,0.866025403784439,1.,0.866025403784439,1.,0.866025403784439,1.,0.866025403784439,
1.,0.866025403784439,1.,0.866025403784439,1.,0.866025403784439,1.,0.866025403784439,
1.,0.866025403784439,1.,0.866025403784439,1.,0.866025403784439,1.,0.866025403784439,
1.,0.866025403784439,1.,0.866025403784439,1.,0.866025403784439,1.,0.866025403784439,
1.,0.866025403784439,1.,0.866025403784439,1.,0.866025403784439,1.,0.866025403784439,
1.,0.866025403784439,1.,0.866025403784439,1.,0.866025403784439,1.,0.866025403784439,
1.,0.866025403784439,1.,0.866025403784439,1.,0.866025403784439,1.,0.866025403784439,
1.,0.866025403784439,1.,0.866025403784439,1.,0.866025403784439,1.,0.866025403784439,
1.,0.866025403784439,1.,0.866025403784439,1.,0.866025403784439,1.,0.866025403784439,
1.,0.866025403784439,1.,0.866025403784439,1.,0.866025403784439,1.,0.866025403784439,
1.,0.866025403784439,1.,0.866025403784439,1.,0.866025403784439,1.,0.866025403784439,
1.,0.866025403784439,1.,0.866025403784439,1.,0.866025403784439,1.,0.866025403784439,
1.,0.866025403784439,1.,0.866025403784439,1.,0.866025403784439,1.,0.866025403784439,
1.,0.866025403784439,1.,0.866025403784439,1.,0.866025403784439,1.,0.866025403784439,
1.,0.866025403784439,1.,0.866025403784439,1.,0.866025403784439,1.,0.866025403784439,
1.,0.866025403784439,1.,0.866025403784439,1.,0.866025403784439,1.)))
REPRESENTATION_ITEM('')
SURFACE()
);
#63=(
BOUNDED_SURFACE()
B_SPLINE_SURFACE(3,2,((#9369,#9370,#9371,#9372,#9373,#9374,#9375,#9376,
#9377,#9378,#9379,#9380,#9381,#9382,#9383,#9384,#9385,#9386,#9387,#9388,
#9389,#9390,#9391,#9392,#9393,#9394,#9395,#9396,#9397,#9398,#9399,#9400,
#9401,#9402,#9403,#9404,#9405,#9406,#9407,#9408,#9409,#9410,#9411,#9412,
#9413,#9414,#9415,#9416,#9417,#9418,#9419,#9420,#9421,#9422,#9423,#9424,
#9425,#9426,#9427,#9428,#9429,#9430,#9431,#9432,#9433,#9434,#9435,#9436,
#9437,#9438,#9439,#9440,#9441,#9442,#9443,#9444,#9445,#9446,#9447,#9448,
#9449,#9450,#9451,#9452,#9453,#9454,#9455,#9456,#9457,#9458,#9459,#9460,
#9461,#9462,#9463,#9464,#9465,#9466,#9467,#9468,#9469,#9470,#9471,#9472,
#9473,#9474,#9475,#9476,#9477,#9478,#9479,#9480,#9481,#9482,#9483,#9484,
#9485,#9486,#9487,#9488,#9489,#9490,#9491,#9492,#9493,#9494,#9495,#9496,
#9497,#9498,#9499,#9500,#9501,#9502,#9503,#9504,#9505,#9506,#9507,#9508,
#9509,#9510,#9511,#9512,#9513,#9514,#9515,#9516,#9517,#9518,#9519,#9520,
#9521,#9522,#9523,#9524,#9525,#9526,#9527,#9528,#9529,#9530,#9531,#9532,
#9533,#9534,#9535,#9536,#9537,#9538,#9539,#9540,#9541,#9542,#9543,#9544,
#9545,#9546,#9547,#9548,#9549,#9550,#9551,#9552,#9553,#9554,#9555,#9556,
#9557,#9558,#9559,#9560,#9561,#9562,#9563,#9564,#9565,#9566,#9567,#9568,
#9569,#9570,#9571,#9572,#9573,#9574,#9575,#9576,#9577,#9578,#9579,#9580,
#9581,#9582,#9583,#9584,#9585,#9586,#9587,#9588,#9589,#9590,#9591,#9592,
#9593,#9594,#9595,#9596,#9597,#9598,#9599,#9600,#9601,#9602,#9603,#9604,
#9605,#9606,#9607,#9608,#9609),(#9610,#9611,#9612,#9613,#9614,#9615,#9616,
#9617,#9618,#9619,#9620,#9621,#9622,#9623,#9624,#9625,#9626,#9627,#9628,
#9629,#9630,#9631,#9632,#9633,#9634,#9635,#9636,#9637,#9638,#9639,#9640,
#9641,#9642,#9643,#9644,#9645,#9646,#9647,#9648,#9649,#9650,#9651,#9652,
#9653,#9654,#9655,#9656,#9657,#9658,#9659,#9660,#9661,#9662,#9663,#9664,
#9665,#9666,#9667,#9668,#9669,#9670,#9671,#9672,#9673,#9674,#9675,#9676,
#9677,#9678,#9679,#9680,#9681,#9682,#9683,#9684,#9685,#9686,#9687,#9688,
#9689,#9690,#9691,#9692,#9693,#9694,#9695,#9696,#9697,#9698,#9699,#9700,
#9701,#9702,#9703,#9704,#9705,#9706,#9707,#9708,#9709,#9710,#9711,#9712,
#9713,#9714,#9715,#9716,#9717,#9718,#9719,#9720,#9721,#9722,#9723,#9724,
#9725,#9726,#9727,#9728,#9729,#9730,#9731,#9732,#9733,#9734,#9735,#9736,
#9737,#9738,#9739,#9740,#9741,#9742,#9743,#9744,#9745,#9746,#9747,#9748,
#9749,#9750,#9751,#9752,#9753,#9754,#9755,#9756,#9757,#9758,#9759,#9760,
#9761,#9762,#9763,#9764,#9765,#9766,#9767,#9768,#9769,#9770,#9771,#9772,
#9773,#9774,#9775,#9776,#9777,#9778,#9779,#9780,#9781,#9782,#9783,#9784,
#9785,#9786,#9787,#9788,#9789,#9790,#9791,#9792,#9793,#9794,#9795,#9796,
#9797,#9798,#9799,#9800,#9801,#9802,#9803,#9804,#9805,#9806,#9807,#9808,
#9809,#9810,#9811,#9812,#9813,#9814,#9815,#9816,#9817,#9818,#9819,#9820,
#9821,#9822,#9823,#9824,#9825,#9826,#9827,#9828,#9829,#9830,#9831,#9832,
#9833,#9834,#9835,#9836,#9837,#9838,#9839,#9840,#9841,#9842,#9843,#9844,
#9845,#9846,#9847,#9848,#9849,#9850),(#9851,#9852,#9853,#9854,#9855,#9856,
#9857,#9858,#9859,#9860,#9861,#9862,#9863,#9864,#9865,#9866,#9867,#9868,
#9869,#9870,#9871,#9872,#9873,#9874,#9875,#9876,#9877,#9878,#9879,#9880,
#9881,#9882,#9883,#9884,#9885,#9886,#9887,#9888,#9889,#9890,#9891,#9892,
#9893,#9894,#9895,#9896,#9897,#9898,#9899,#9900,#9901,#9902,#9903,#9904,
#9905,#9906,#9907,#9908,#9909,#9910,#9911,#9912,#9913,#9914,#9915,#9916,
#9917,#9918,#9919,#9920,#9921,#9922,#9923,#9924,#9925,#9926,#9927,#9928,
#9929,#9930,#9931,#9932,#9933,#9934,#9935,#9936,#9937,#9938,#9939,#9940,
#9941,#9942,#9943,#9944,#9945,#9946,#9947,#9948,#9949,#9950,#9951,#9952,
#9953,#9954,#9955,#9956,#9957,#9958,#9959,#9960,#9961,#9962,#9963,#9964,
#9965,#9966,#9967,#9968,#9969,#9970,#9971,#9972,#9973,#9974,#9975,#9976,
#9977,#9978,#9979,#9980,#9981,#9982,#9983,#9984,#9985,#9986,#9987,#9988,
#9989,#9990,#9991,#9992,#9993,#9994,#9995,#9996,#9997,#9998,#9999,#10000,
#10001,#10002,#10003,#10004,#10005,#10006,#10007,#10008,#10009,#10010,#10011,
#10012,#10013,#10014,#10015,#10016,#10017,#10018,#10019,#10020,#10021,#10022,
#10023,#10024,#10025,#10026,#10027,#10028,#10029,#10030,#10031,#10032,#10033,
#10034,#10035,#10036,#10037,#10038,#10039,#10040,#10041,#10042,#10043,#10044,
#10045,#10046,#10047,#10048,#10049,#10050,#10051,#10052,#10053,#10054,#10055,
#10056,#10057,#10058,#10059,#10060,#10061,#10062,#10063,#10064,#10065,#10066,
#10067,#10068,#10069,#10070,#10071,#10072,#10073,#10074,#10075,#10076,#10077,
#10078,#10079,#10080,#10081,#10082,#10083,#10084,#10085,#10086,#10087,#10088,
#10089,#10090,#10091),(#10092,#10093,#10094,#10095,#10096,#10097,#10098,
#10099,#10100,#10101,#10102,#10103,#10104,#10105,#10106,#10107,#10108,#10109,
#10110,#10111,#10112,#10113,#10114,#10115,#10116,#10117,#10118,#10119,#10120,
#10121,#10122,#10123,#10124,#10125,#10126,#10127,#10128,#10129,#10130,#10131,
#10132,#10133,#10134,#10135,#10136,#10137,#10138,#10139,#10140,#10141,#10142,
#10143,#10144,#10145,#10146,#10147,#10148,#10149,#10150,#10151,#10152,#10153,
#10154,#10155,#10156,#10157,#10158,#10159,#10160,#10161,#10162,#10163,#10164,
#10165,#10166,#10167,#10168,#10169,#10170,#10171,#10172,#10173,#10174,#10175,
#10176,#10177,#10178,#10179,#10180,#10181,#10182,#10183,#10184,#10185,#10186,
#10187,#10188,#10189,#10190,#10191,#10192,#10193,#10194,#10195,#10196,#10197,
#10198,#10199,#10200,#10201,#10202,#10203,#10204,#10205,#10206,#10207,#10208,
#10209,#10210,#10211,#10212,#10213,#10214,#10215,#10216,#10217,#10218,#10219,
#10220,#10221,#10222,#10223,#10224,#10225,#10226,#10227,#10228,#10229,#10230,
#10231,#10232,#10233,#10234,#10235,#10236,#10237,#10238,#10239,#10240,#10241,
#10242,#10243,#10244,#10245,#10246,#10247,#10248,#10249,#10250,#10251,#10252,
#10253,#10254,#10255,#10256,#10257,#10258,#10259,#10260,#10261,#10262,#10263,
#10264,#10265,#10266,#10267,#10268,#10269,#10270,#10271,#10272,#10273,#10274,
#10275,#10276,#10277,#10278,#10279,#10280,#10281,#10282,#10283,#10284,#10285,
#10286,#10287,#10288,#10289,#10290,#10291,#10292,#10293,#10294,#10295,#10296,
#10297,#10298,#10299,#10300,#10301,#10302,#10303,#10304,#10305,#10306,#10307,
#10308,#10309,#10310,#10311,#10312,#10313,#10314,#10315,#10316,#10317,#10318,
#10319,#10320,#10321,#10322,#10323,#10324,#10325,#10326,#10327,#10328,#10329,
#10330,#10331,#10332),(#10333,#10334,#10335,#10336,#10337,#10338,#10339,
#10340,#10341,#10342,#10343,#10344,#10345,#10346,#10347,#10348,#10349,#10350,
#10351,#10352,#10353,#10354,#10355,#10356,#10357,#10358,#10359,#10360,#10361,
#10362,#10363,#10364,#10365,#10366,#10367,#10368,#10369,#10370,#10371,#10372,
#10373,#10374,#10375,#10376,#10377,#10378,#10379,#10380,#10381,#10382,#10383,
#10384,#10385,#10386,#10387,#10388,#10389,#10390,#10391,#10392,#10393,#10394,
#10395,#10396,#10397,#10398,#10399,#10400,#10401,#10402,#10403,#10404,#10405,
#10406,#10407,#10408,#10409,#10410,#10411,#10412,#10413,#10414,#10415,#10416,
#10417,#10418,#10419,#10420,#10421,#10422,#10423,#10424,#10425,#10426,#10427,
#10428,#10429,#10430,#10431,#10432,#10433,#10434,#10435,#10436,#10437,#10438,
#10439,#10440,#10441,#10442,#10443,#10444,#10445,#10446,#10447,#10448,#10449,
#10450,#10451,#10452,#10453,#10454,#10455,#10456,#10457,#10458,#10459,#10460,
#10461,#10462,#10463,#10464,#10465,#10466,#10467,#10468,#10469,#10470,#10471,
#10472,#10473,#10474,#10475,#10476,#10477,#10478,#10479,#10480,#10481,#10482,
#10483,#10484,#10485,#10486,#10487,#10488,#10489,#10490,#10491,#10492,#10493,
#10494,#10495,#10496,#10497,#10498,#10499,#10500,#10501,#10502,#10503,#10504,
#10505,#10506,#10507,#10508,#10509,#10510,#10511,#10512,#10513,#10514,#10515,
#10516,#10517,#10518,#10519,#10520,#10521,#10522,#10523,#10524,#10525,#10526,
#10527,#10528,#10529,#10530,#10531,#10532,#10533,#10534,#10535,#10536,#10537,
#10538,#10539,#10540,#10541,#10542,#10543,#10544,#10545,#10546,#10547,#10548,
#10549,#10550,#10551,#10552,#10553,#10554,#10555,#10556,#10557,#10558,#10559,
#10560,#10561,#10562,#10563,#10564,#10565,#10566,#10567,#10568,#10569,#10570,
#10571,#10572,#10573),(#10574,#10575,#10576,#10577,#10578,#10579,#10580,
#10581,#10582,#10583,#10584,#10585,#10586,#10587,#10588,#10589,#10590,#10591,
#10592,#10593,#10594,#10595,#10596,#10597,#10598,#10599,#10600,#10601,#10602,
#10603,#10604,#10605,#10606,#10607,#10608,#10609,#10610,#10611,#10612,#10613,
#10614,#10615,#10616,#10617,#10618,#10619,#10620,#10621,#10622,#10623,#10624,
#10625,#10626,#10627,#10628,#10629,#10630,#10631,#10632,#10633,#10634,#10635,
#10636,#10637,#10638,#10639,#10640,#10641,#10642,#10643,#10644,#10645,#10646,
#10647,#10648,#10649,#10650,#10651,#10652,#10653,#10654,#10655,#10656,#10657,
#10658,#10659,#10660,#10661,#10662,#10663,#10664,#10665,#10666,#10667,#10668,
#10669,#10670,#10671,#10672,#10673,#10674,#10675,#10676,#10677,#10678,#10679,
#10680,#10681,#10682,#10683,#10684,#10685,#10686,#10687,#10688,#10689,#10690,
#10691,#10692,#10693,#10694,#10695,#10696,#10697,#10698,#10699,#10700,#10701,
#10702,#10703,#10704,#10705,#10706,#10707,#10708,#10709,#10710,#10711,#10712,
#10713,#10714,#10715,#10716,#10717,#10718,#10719,#10720,#10721,#10722,#10723,
#10724,#10725,#10726,#10727,#10728,#10729,#10730,#10731,#10732,#10733,#10734,
#10735,#10736,#10737,#10738,#10739,#10740,#10741,#10742,#10743,#10744,#10745,
#10746,#10747,#10748,#10749,#10750,#10751,#10752,#10753,#10754,#10755,#10756,
#10757,#10758,#10759,#10760,#10761,#10762,#10763,#10764,#10765,#10766,#10767,
#10768,#10769,#10770,#10771,#10772,#10773,#10774,#10775,#10776,#10777,#10778,
#10779,#10780,#10781,#10782,#10783,#10784,#10785,#10786,#10787,#10788,#10789,
#10790,#10791,#10792,#10793,#10794,#10795,#10796,#10797,#10798,#10799,#10800,
#10801,#10802,#10803,#10804,#10805,#10806,#10807,#10808,#10809,#10810,#10811,
#10812,#10813,#10814),(#10815,#10816,#10817,#10818,#10819,#10820,#10821,
#10822,#10823,#10824,#10825,#10826,#10827,#10828,#10829,#10830,#10831,#10832,
#10833,#10834,#10835,#10836,#10837,#10838,#10839,#10840,#10841,#10842,#10843,
#10844,#10845,#10846,#10847,#10848,#10849,#10850,#10851,#10852,#10853,#10854,
#10855,#10856,#10857,#10858,#10859,#10860,#10861,#10862,#10863,#10864,#10865,
#10866,#10867,#10868,#10869,#10870,#10871,#10872,#10873,#10874,#10875,#10876,
#10877,#10878,#10879,#10880,#10881,#10882,#10883,#10884,#10885,#10886,#10887,
#10888,#10889,#10890,#10891,#10892,#10893,#10894,#10895,#10896,#10897,#10898,
#10899,#10900,#10901,#10902,#10903,#10904,#10905,#10906,#10907,#10908,#10909,
#10910,#10911,#10912,#10913,#10914,#10915,#10916,#10917,#10918,#10919,#10920,
#10921,#10922,#10923,#10924,#10925,#10926,#10927,#10928,#10929,#10930,#10931,
#10932,#10933,#10934,#10935,#10936,#10937,#10938,#10939,#10940,#10941,#10942,
#10943,#10944,#10945,#10946,#10947,#10948,#10949,#10950,#10951,#10952,#10953,
#10954,#10955,#10956,#10957,#10958,#10959,#10960,#10961,#10962,#10963,#10964,
#10965,#10966,#10967,#10968,#10969,#10970,#10971,#10972,#10973,#10974,#10975,
#10976,#10977,#10978,#10979,#10980,#10981,#10982,#10983,#10984,#10985,#10986,
#10987,#10988,#10989,#10990,#10991,#10992,#10993,#10994,#10995,#10996,#10997,
#10998,#10999,#11000,#11001,#11002,#11003,#11004,#11005,#11006,#11007,#11008,
#11009,#11010,#11011,#11012,#11013,#11014,#11015,#11016,#11017,#11018,#11019,
#11020,#11021,#11022,#11023,#11024,#11025,#11026,#11027,#11028,#11029,#11030,
#11031,#11032,#11033,#11034,#11035,#11036,#11037,#11038,#11039,#11040,#11041,
#11042,#11043,#11044,#11045,#11046,#11047,#11048,#11049,#11050,#11051,#11052,
#11053,#11054,#11055)),.UNSPECIFIED.,.T.,.F.,.F.)
B_SPLINE_SURFACE_WITH_KNOTS((4,3,4),(3,2,2,2,2,2,2,2,2,2,2,2,2,2,2,2,2,
2,2,2,2,2,2,2,2,2,2,2,2,2,2,2,2,2,2,2,2,2,2,2,2,2,2,2,2,2,2,2,2,2,2,2,2,
2,2,2,2,2,2,2,2,2,2,2,2,2,2,2,2,2,2,2,2,2,2,2,2,2,2,2,2,2,2,2,2,2,2,2,2,
2,2,2,2,2,2,2,2,2,2,2,2,2,2,2,2,2,2,2,2,2,2,2,2,2,2,2,2,2,2,2,3),(0.,0.5,
1.),(0.,0.00833333333333333,0.0166666666666667,0.025,0.0333333333333333,
0.0416666666666667,0.05,0.0583333333333333,0.0666666666666667,0.075,0.0833333333333333,
0.0916666666666667,0.1,0.108333333333333,0.116666666666667,0.125,0.133333333333333,
0.141666666666667,0.15,0.158333333333333,0.166666666666667,0.175,0.183333333333333,
0.191666666666667,0.2,0.208333333333333,0.216666666666667,0.225,0.233333333333333,
0.241666666666667,0.25,0.258333333333333,0.266666666666667,0.275,0.283333333333333,
0.291666666666667,0.3,0.308333333333333,0.316666666666667,0.325,0.333333333333333,
0.341666666666667,0.35,0.358333333333333,0.366666666666667,0.375,0.383333333333333,
0.391666666666667,0.4,0.408333333333333,0.416666666666667,0.425,0.433333333333333,
0.441666666666667,0.45,0.458333333333333,0.466666666666667,0.475,0.483333333333333,
0.491666666666667,0.5,0.508333333333333,0.516666666666667,0.525,0.533333333333333,
0.541666666666667,0.55,0.558333333333333,0.566666666666667,0.575,0.583333333333333,
0.591666666666667,0.6,0.608333333333333,0.616666666666667,0.625,0.633333333333333,
0.641666666666667,0.65,0.658333333333333,0.666666666666667,0.675,0.683333333333333,
0.691666666666667,0.7,0.708333333333333,0.716666666666667,0.725,0.733333333333333,
0.741666666666667,0.75,0.758333333333333,0.766666666666667,0.775,0.783333333333333,
0.791666666666667,0.8,0.808333333333333,0.816666666666667,0.825,0.833333333333333,
0.841666666666667,0.85,0.858333333333333,0.866666666666667,0.875,0.883333333333333,
0.891666666666667,0.9,0.908333333333333,0.916666666666667,0.925,0.933333333333333,
0.941666666666667,0.95,0.958333333333333,0.966666666666667,0.975,0.983333333333333,
0.991666666666667,1.),.UNSPECIFIED.)
GEOMETRIC_REPRESENTATION_ITEM()
RATIONAL_B_SPLINE_SURFACE(((1.,0.965925826289068,1.,0.965925826289068,1.,
0.965925826289068,1.,0.965925826289068,1.,0.965925826289068,1.,0.965925826289068,
1.,0.965925826289068,1.,0.965925826289068,1.,0.965925826289068,1.,0.965925826289068,
1.,0.965925826289068,1.,0.965925826289068,1.,0.965925826289068,1.,0.965925826289068,
1.,0.965925826289068,1.,0.965925826289068,1.,0.965925826289068,1.,0.965925826289068,
1.,0.965925826289068,1.,0.965925826289068,1.,0.965925826289068,1.,0.965925826289068,
1.,0.965925826289068,1.,0.965925826289068,1.,0.965925826289068,1.,0.965925826289068,
1.,0.965925826289068,1.,0.965925826289068,1.,0.965925826289068,1.,0.965925826289068,
1.,0.965925826289068,1.,0.965925826289068,1.,0.965925826289068,1.,0.965925826289068,
1.,0.965925826289068,1.,0.965925826289068,1.,0.965925826289068,1.,0.965925826289068,
1.,0.965925826289068,1.,0.965925826289068,1.,0.965925826289068,1.,0.965925826289068,
1.,0.965925826289068,1.,0.965925826289068,1.,0.965925826289068,1.,0.965925826289068,
1.,0.965925826289068,1.,0.965925826289068,1.,0.965925826289068,1.,0.965925826289068,
1.,0.965925826289068,1.,0.965925826289068,1.,0.965925826289068,1.,0.965925826289068,
1.,0.965925826289068,1.,0.965925826289068,1.,0.965925826289068,1.,0.965925826289068,
1.,0.965925826289068,1.,0.965925826289068,1.,0.965925826289068,1.,0.965925826289068,
1.,0.965925826289068,1.,0.965925826289068,1.,0.965925826289068,1.,0.965925826289068,
1.,0.965925826289068,1.,0.965925826289068,1.,0.965925826289068,1.,0.965925826289068,
1.,0.965925826289068,1.,0.965925826289068,1.,0.965925826289068,1.,0.965925826289068,
1.,0.965925826289068,1.,0.965925826289068,1.,0.965925826289068,1.,0.965925826289068,
1.,0.965925826289068,1.,0.965925826289068,1.,0.965925826289068,1.,0.965925826289068,
1.,0.965925826289068,1.,0.965925826289068,1.,0.965925826289068,1.,0.965925826289068,
1.,0.965925826289068,1.,0.965925826289068,1.,0.965925826289068,1.,0.965925826289068,
1.,0.965925826289068,1.,0.965925826289068,1.,0.965925826289068,1.,0.965925826289068,
1.,0.965925826289068,1.,0.965925826289068,1.,0.965925826289068,1.,0.965925826289068,
1.,0.965925826289068,1.,0.965925826289068,1.,0.965925826289068,1.,0.965925826289068,
1.,0.965925826289068,1.,0.965925826289068,1.,0.965925826289068,1.,0.965925826289068,
1.,0.965925826289068,1.,0.965925826289068,1.,0.965925826289068,1.,0.965925826289068,
1.,0.965925826289068,1.,0.965925826289068,1.,0.965925826289068,1.,0.965925826289068,
1.,0.965925826289068,1.,0.965925826289068,1.,0.965925826289068,1.,0.965925826289068,
1.,0.965925826289068,1.,0.965925826289068,1.),(0.333333333333333,0.321975275429689,
0.333333333333333,0.321975275429689,0.333333333333333,0.321975275429689,
0.333333333333333,0.321975275429689,0.333333333333333,0.321975275429689,
0.333333333333333,0.321975275429689,0.333333333333333,0.321975275429689,
0.333333333333333,0.321975275429689,0.333333333333333,0.321975275429689,
0.333333333333333,0.321975275429689,0.333333333333333,0.321975275429689,
0.333333333333333,0.321975275429689,0.333333333333333,0.321975275429689,
0.333333333333333,0.321975275429689,0.333333333333333,0.321975275429689,
0.333333333333333,0.321975275429689,0.333333333333333,0.321975275429689,
0.333333333333333,0.321975275429689,0.333333333333333,0.321975275429689,
0.333333333333333,0.321975275429689,0.333333333333333,0.321975275429689,
0.333333333333333,0.321975275429689,0.333333333333333,0.321975275429689,
0.333333333333333,0.321975275429689,0.333333333333333,0.321975275429689,
0.333333333333333,0.321975275429689,0.333333333333333,0.321975275429689,
0.333333333333333,0.321975275429689,0.333333333333333,0.321975275429689,
0.333333333333333,0.321975275429689,0.333333333333333,0.321975275429689,
0.333333333333333,0.321975275429689,0.333333333333333,0.321975275429689,
0.333333333333333,0.321975275429689,0.333333333333333,0.321975275429689,
0.333333333333333,0.321975275429689,0.333333333333333,0.321975275429689,
0.333333333333333,0.321975275429689,0.333333333333333,0.321975275429689,
0.333333333333333,0.321975275429689,0.333333333333333,0.321975275429689,
0.333333333333333,0.321975275429689,0.333333333333333,0.321975275429689,
0.333333333333333,0.321975275429689,0.333333333333333,0.321975275429689,
0.333333333333333,0.321975275429689,0.333333333333333,0.321975275429689,
0.333333333333333,0.321975275429689,0.333333333333333,0.321975275429689,
0.333333333333333,0.321975275429689,0.333333333333333,0.321975275429689,
0.333333333333333,0.321975275429689,0.333333333333333,0.321975275429689,
0.333333333333333,0.321975275429689,0.333333333333333,0.321975275429689,
0.333333333333333,0.321975275429689,0.333333333333333,0.321975275429689,
0.333333333333333,0.321975275429689,0.333333333333333,0.321975275429689,
0.333333333333333,0.321975275429689,0.333333333333333,0.321975275429689,
0.333333333333333,0.321975275429689,0.333333333333333,0.321975275429689,
0.333333333333333,0.321975275429689,0.333333333333333,0.321975275429689,
0.333333333333333,0.321975275429689,0.333333333333333,0.321975275429689,
0.333333333333333,0.321975275429689,0.333333333333333,0.321975275429689,
0.333333333333333,0.321975275429689,0.333333333333333,0.321975275429689,
0.333333333333333,0.321975275429689,0.333333333333333,0.321975275429689,
0.333333333333333,0.321975275429689,0.333333333333333,0.321975275429689,
0.333333333333333,0.321975275429689,0.333333333333333,0.321975275429689,
0.333333333333333,0.321975275429689,0.333333333333333,0.321975275429689,
0.333333333333333,0.321975275429689,0.333333333333333,0.321975275429689,
0.333333333333333,0.321975275429689,0.333333333333333,0.321975275429689,
0.333333333333333,0.321975275429689,0.333333333333333,0.321975275429689,
0.333333333333333,0.321975275429689,0.333333333333333,0.321975275429689,
0.333333333333333,0.321975275429689,0.333333333333333,0.321975275429689,
0.333333333333333,0.321975275429689,0.333333333333333,0.321975275429689,
0.333333333333333,0.321975275429689,0.333333333333333,0.321975275429689,
0.333333333333333,0.321975275429689,0.333333333333333,0.321975275429689,
0.333333333333333,0.321975275429689,0.333333333333333,0.321975275429689,
0.333333333333333,0.321975275429689,0.333333333333333,0.321975275429689,
0.333333333333333,0.321975275429689,0.333333333333333,0.321975275429689,
0.333333333333333,0.321975275429689,0.333333333333333,0.321975275429689,
0.333333333333333,0.321975275429689,0.333333333333333,0.321975275429689,
0.333333333333333,0.321975275429689,0.333333333333333,0.321975275429689,
0.333333333333333,0.321975275429689,0.333333333333333,0.321975275429689,
0.333333333333333,0.321975275429689,0.333333333333333,0.321975275429689,
0.333333333333333,0.321975275429689,0.333333333333333,0.321975275429689,
0.333333333333333,0.321975275429689,0.333333333333333,0.321975275429689,
0.333333333333333,0.321975275429689,0.333333333333333,0.321975275429689,
0.333333333333333,0.321975275429689,0.333333333333333,0.321975275429689,
0.333333333333333,0.321975275429689,0.333333333333333),(0.333333333333333,
0.321975275429689,0.333333333333333,0.321975275429689,0.333333333333333,
0.321975275429689,0.333333333333333,0.321975275429689,0.333333333333333,
0.321975275429689,0.333333333333333,0.321975275429689,0.333333333333333,
0.321975275429689,0.333333333333333,0.321975275429689,0.333333333333333,
0.321975275429689,0.333333333333333,0.321975275429689,0.333333333333333,
0.321975275429689,0.333333333333333,0.321975275429689,0.333333333333333,
0.321975275429689,0.333333333333333,0.321975275429689,0.333333333333333,
0.321975275429689,0.333333333333333,0.321975275429689,0.333333333333333,
0.321975275429689,0.333333333333333,0.321975275429689,0.333333333333333,
0.321975275429689,0.333333333333333,0.321975275429689,0.333333333333333,
0.321975275429689,0.333333333333333,0.321975275429689,0.333333333333333,
0.321975275429689,0.333333333333333,0.321975275429689,0.333333333333333,
0.321975275429689,0.333333333333333,0.321975275429689,0.333333333333333,
0.321975275429689,0.333333333333333,0.321975275429689,0.333333333333333,
0.321975275429689,0.333333333333333,0.321975275429689,0.333333333333333,
0.321975275429689,0.333333333333333,0.321975275429689,0.333333333333333,
0.321975275429689,0.333333333333333,0.321975275429689,0.333333333333333,
0.321975275429689,0.333333333333333,0.321975275429689,0.333333333333333,
0.321975275429689,0.333333333333333,0.321975275429689,0.333333333333333,
0.321975275429689,0.333333333333333,0.321975275429689,0.333333333333333,
0.321975275429689,0.333333333333333,0.321975275429689,0.333333333333333,
0.321975275429689,0.333333333333333,0.321975275429689,0.333333333333333,
0.321975275429689,0.333333333333333,0.321975275429689,0.333333333333333,
0.321975275429689,0.333333333333333,0.321975275429689,0.333333333333333,
0.321975275429689,0.333333333333333,0.321975275429689,0.333333333333333,
0.321975275429689,0.333333333333333,0.321975275429689,0.333333333333333,
0.321975275429689,0.333333333333333,0.321975275429689,0.333333333333333,
0.321975275429689,0.333333333333333,0.321975275429689,0.333333333333333,
0.321975275429689,0.333333333333333,0.321975275429689,0.333333333333333,
0.321975275429689,0.333333333333333,0.321975275429689,0.333333333333333,
0.321975275429689,0.333333333333333,0.321975275429689,0.333333333333333,
0.321975275429689,0.333333333333333,0.321975275429689,0.333333333333333,
0.321975275429689,0.333333333333333,0.321975275429689,0.333333333333333,
0.321975275429689,0.333333333333333,0.321975275429689,0.333333333333333,
0.321975275429689,0.333333333333333,0.321975275429689,0.333333333333333,
0.321975275429689,0.333333333333333,0.321975275429689,0.333333333333333,
0.321975275429689,0.333333333333333,0.321975275429689,0.333333333333333,
0.321975275429689,0.333333333333333,0.321975275429689,0.333333333333333,
0.321975275429689,0.333333333333333,0.321975275429689,0.333333333333333,
0.321975275429689,0.333333333333333,0.321975275429689,0.333333333333333,
0.321975275429689,0.333333333333333,0.321975275429689,0.333333333333333,
0.321975275429689,0.333333333333333,0.321975275429689,0.333333333333333,
0.321975275429689,0.333333333333333,0.321975275429689,0.333333333333333,
0.321975275429689,0.333333333333333,0.321975275429689,0.333333333333333,
0.321975275429689,0.333333333333333,0.321975275429689,0.333333333333333,
0.321975275429689,0.333333333333333,0.321975275429689,0.333333333333333,
0.321975275429689,0.333333333333333,0.321975275429689,0.333333333333333,
0.321975275429689,0.333333333333333,0.321975275429689,0.333333333333333,
0.321975275429689,0.333333333333333,0.321975275429689,0.333333333333333,
0.321975275429689,0.333333333333333,0.321975275429689,0.333333333333333,
0.321975275429689,0.333333333333333,0.321975275429689,0.333333333333333,
0.321975275429689,0.333333333333333,0.321975275429689,0.333333333333333,
0.321975275429689,0.333333333333333,0.321975275429689,0.333333333333333,
0.321975275429689,0.333333333333333,0.321975275429689,0.333333333333333,
0.321975275429689,0.333333333333333,0.321975275429689,0.333333333333333,
0.321975275429689,0.333333333333333,0.321975275429689,0.333333333333333,
0.321975275429689,0.333333333333333,0.321975275429689,0.333333333333333,
0.321975275429689,0.333333333333333,0.321975275429689,0.333333333333333,
0.321975275429689,0.333333333333333,0.321975275429689,0.333333333333333,
0.321975275429689,0.333333333333333,0.321975275429689,0.333333333333333),
(1.,0.965925826289068,1.,0.965925826289068,1.,0.965925826289068,1.,0.965925826289068,
1.,0.965925826289068,1.,0.965925826289068,1.,0.965925826289068,1.,0.965925826289068,
1.,0.965925826289068,1.,0.965925826289068,1.,0.965925826289068,1.,0.965925826289068,
1.,0.965925826289068,1.,0.965925826289068,1.,0.965925826289068,1.,0.965925826289068,
1.,0.965925826289068,1.,0.965925826289068,1.,0.965925826289068,1.,0.965925826289068,
1.,0.965925826289068,1.,0.965925826289068,1.,0.965925826289068,1.,0.965925826289068,
1.,0.965925826289068,1.,0.965925826289068,1.,0.965925826289068,1.,0.965925826289068,
1.,0.965925826289068,1.,0.965925826289068,1.,0.965925826289068,1.,0.965925826289068,
1.,0.965925826289068,1.,0.965925826289068,1.,0.965925826289068,1.,0.965925826289068,
1.,0.965925826289068,1.,0.965925826289068,1.,0.965925826289068,1.,0.965925826289068,
1.,0.965925826289068,1.,0.965925826289068,1.,0.965925826289068,1.,0.965925826289068,
1.,0.965925826289068,1.,0.965925826289068,1.,0.965925826289068,1.,0.965925826289068,
1.,0.965925826289068,1.,0.965925826289068,1.,0.965925826289068,1.,0.965925826289068,
1.,0.965925826289068,1.,0.965925826289068,1.,0.965925826289068,1.,0.965925826289068,
1.,0.965925826289068,1.,0.965925826289068,1.,0.965925826289068,1.,0.965925826289068,
1.,0.965925826289068,1.,0.965925826289068,1.,0.965925826289068,1.,0.965925826289068,
1.,0.965925826289068,1.,0.965925826289068,1.,0.965925826289068,1.,0.965925826289068,
1.,0.965925826289068,1.,0.965925826289068,1.,0.965925826289068,1.,0.965925826289068,
1.,0.965925826289068,1.,0.965925826289068,1.,0.965925826289068,1.,0.965925826289068,
1.,0.965925826289068,1.,0.965925826289068,1.,0.965925826289068,1.,0.965925826289068,
1.,0.965925826289068,1.,0.965925826289068,1.,0.965925826289068,1.,0.965925826289068,
1.,0.965925826289068,1.,0.965925826289068,1.,0.965925826289068,1.,0.965925826289068,
1.,0.965925826289068,1.,0.965925826289068,1.,0.965925826289068,1.,0.965925826289068,
1.,0.965925826289068,1.,0.965925826289068,1.,0.965925826289068,1.,0.965925826289068,
1.,0.965925826289068,1.,0.965925826289068,1.,0.965925826289068,1.,0.965925826289068,
1.,0.965925826289068,1.,0.965925826289068,1.,0.965925826289068,1.,0.965925826289068,
1.,0.965925826289068,1.,0.965925826289068,1.,0.965925826289068,1.,0.965925826289068,
1.,0.965925826289068,1.,0.965925826289068,1.,0.965925826289068,1.,0.965925826289068,
1.,0.965925826289068,1.,0.965925826289068,1.,0.965925826289068,1.,0.965925826289068,
1.,0.965925826289068,1.,0.965925826289068,1.,0.965925826289068,1.,0.965925826289068,
1.),(0.333333333333333,0.321975275429689,0.333333333333333,0.321975275429689,
0.333333333333333,0.321975275429689,0.333333333333333,0.321975275429689,
0.333333333333333,0.321975275429689,0.333333333333333,0.321975275429689,
0.333333333333333,0.321975275429689,0.333333333333333,0.321975275429689,
0.333333333333333,0.321975275429689,0.333333333333333,0.321975275429689,
0.333333333333333,0.321975275429689,0.333333333333333,0.321975275429689,
0.333333333333333,0.321975275429689,0.333333333333333,0.321975275429689,
0.333333333333333,0.321975275429689,0.333333333333333,0.321975275429689,
0.333333333333333,0.321975275429689,0.333333333333333,0.321975275429689,
0.333333333333333,0.321975275429689,0.333333333333333,0.321975275429689,
0.333333333333333,0.321975275429689,0.333333333333333,0.321975275429689,
0.333333333333333,0.321975275429689,0.333333333333333,0.321975275429689,
0.333333333333333,0.321975275429689,0.333333333333333,0.321975275429689,
0.333333333333333,0.321975275429689,0.333333333333333,0.321975275429689,
0.333333333333333,0.321975275429689,0.333333333333333,0.321975275429689,
0.333333333333333,0.321975275429689,0.333333333333333,0.321975275429689,
0.333333333333333,0.321975275429689,0.333333333333333,0.321975275429689,
0.333333333333333,0.321975275429689,0.333333333333333,0.321975275429689,
0.333333333333333,0.321975275429689,0.333333333333333,0.321975275429689,
0.333333333333333,0.321975275429689,0.333333333333333,0.321975275429689,
0.333333333333333,0.321975275429689,0.333333333333333,0.321975275429689,
0.333333333333333,0.321975275429689,0.333333333333333,0.321975275429689,
0.333333333333333,0.321975275429689,0.333333333333333,0.321975275429689,
0.333333333333333,0.321975275429689,0.333333333333333,0.321975275429689,
0.333333333333333,0.321975275429689,0.333333333333333,0.321975275429689,
0.333333333333333,0.321975275429689,0.333333333333333,0.321975275429689,
0.333333333333333,0.321975275429689,0.333333333333333,0.321975275429689,
0.333333333333333,0.321975275429689,0.333333333333333,0.321975275429689,
0.333333333333333,0.321975275429689,0.333333333333333,0.321975275429689,
0.333333333333333,0.321975275429689,0.333333333333333,0.321975275429689,
0.333333333333333,0.321975275429689,0.333333333333333,0.321975275429689,
0.333333333333333,0.321975275429689,0.333333333333333,0.321975275429689,
0.333333333333333,0.321975275429689,0.333333333333333,0.321975275429689,
0.333333333333333,0.321975275429689,0.333333333333333,0.321975275429689,
0.333333333333333,0.321975275429689,0.333333333333333,0.321975275429689,
0.333333333333333,0.321975275429689,0.333333333333333,0.321975275429689,
0.333333333333333,0.321975275429689,0.333333333333333,0.321975275429689,
0.333333333333333,0.321975275429689,0.333333333333333,0.321975275429689,
0.333333333333333,0.321975275429689,0.333333333333333,0.321975275429689,
0.333333333333333,0.321975275429689,0.333333333333333,0.321975275429689,
0.333333333333333,0.321975275429689,0.333333333333333,0.321975275429689,
0.333333333333333,0.321975275429689,0.333333333333333,0.321975275429689,
0.333333333333333,0.321975275429689,0.333333333333333,0.321975275429689,
0.333333333333333,0.321975275429689,0.333333333333333,0.321975275429689,
0.333333333333333,0.321975275429689,0.333333333333333,0.321975275429689,
0.333333333333333,0.321975275429689,0.333333333333333,0.321975275429689,
0.333333333333333,0.321975275429689,0.333333333333333,0.321975275429689,
0.333333333333333,0.321975275429689,0.333333333333333,0.321975275429689,
0.333333333333333,0.321975275429689,0.333333333333333,0.321975275429689,
0.333333333333333,0.321975275429689,0.333333333333333,0.321975275429689,
0.333333333333333,0.321975275429689,0.333333333333333,0.321975275429689,
0.333333333333333,0.321975275429689,0.333333333333333,0.321975275429689,
0.333333333333333,0.321975275429689,0.333333333333333,0.321975275429689,
0.333333333333333,0.321975275429689,0.333333333333333,0.321975275429689,
0.333333333333333,0.321975275429689,0.333333333333333,0.321975275429689,
0.333333333333333,0.321975275429689,0.333333333333333,0.321975275429689,
0.333333333333333,0.321975275429689,0.333333333333333,0.321975275429689,
0.333333333333333,0.321975275429689,0.333333333333333,0.321975275429689,
0.333333333333333,0.321975275429689,0.333333333333333,0.321975275429689,
0.333333333333333,0.321975275429689,0.333333333333333,0.321975275429689,
0.333333333333333),(0.333333333333333,0.321975275429689,0.333333333333333,
0.321975275429689,0.333333333333333,0.321975275429689,0.333333333333333,
0.321975275429689,0.333333333333333,0.321975275429689,0.333333333333333,
0.321975275429689,0.333333333333333,0.321975275429689,0.333333333333333,
0.321975275429689,0.333333333333333,0.321975275429689,0.333333333333333,
0.321975275429689,0.333333333333333,0.321975275429689,0.333333333333333,
0.321975275429689,0.333333333333333,0.321975275429689,0.333333333333333,
0.321975275429689,0.333333333333333,0.321975275429689,0.333333333333333,
0.321975275429689,0.333333333333333,0.321975275429689,0.333333333333333,
0.321975275429689,0.333333333333333,0.321975275429689,0.333333333333333,
0.321975275429689,0.333333333333333,0.321975275429689,0.333333333333333,
0.321975275429689,0.333333333333333,0.321975275429689,0.333333333333333,
0.321975275429689,0.333333333333333,0.321975275429689,0.333333333333333,
0.321975275429689,0.333333333333333,0.321975275429689,0.333333333333333,
0.321975275429689,0.333333333333333,0.321975275429689,0.333333333333333,
0.321975275429689,0.333333333333333,0.321975275429689,0.333333333333333,
0.321975275429689,0.333333333333333,0.321975275429689,0.333333333333333,
0.321975275429689,0.333333333333333,0.321975275429689,0.333333333333333,
0.321975275429689,0.333333333333333,0.321975275429689,0.333333333333333,
0.321975275429689,0.333333333333333,0.321975275429689,0.333333333333333,
0.321975275429689,0.333333333333333,0.321975275429689,0.333333333333333,
0.321975275429689,0.333333333333333,0.321975275429689,0.333333333333333,
0.321975275429689,0.333333333333333,0.321975275429689,0.333333333333333,
0.321975275429689,0.333333333333333,0.321975275429689,0.333333333333333,
0.321975275429689,0.333333333333333,0.321975275429689,0.333333333333333,
0.321975275429689,0.333333333333333,0.321975275429689,0.333333333333333,
0.321975275429689,0.333333333333333,0.321975275429689,0.333333333333333,
0.321975275429689,0.333333333333333,0.321975275429689,0.333333333333333,
0.321975275429689,0.333333333333333,0.321975275429689,0.333333333333333,
0.321975275429689,0.333333333333333,0.321975275429689,0.333333333333333,
0.321975275429689,0.333333333333333,0.321975275429689,0.333333333333333,
0.321975275429689,0.333333333333333,0.321975275429689,0.333333333333333,
0.321975275429689,0.333333333333333,0.321975275429689,0.333333333333333,
0.321975275429689,0.333333333333333,0.321975275429689,0.333333333333333,
0.321975275429689,0.333333333333333,0.321975275429689,0.333333333333333,
0.321975275429689,0.333333333333333,0.321975275429689,0.333333333333333,
0.321975275429689,0.333333333333333,0.321975275429689,0.333333333333333,
0.321975275429689,0.333333333333333,0.321975275429689,0.333333333333333,
0.321975275429689,0.333333333333333,0.321975275429689,0.333333333333333,
0.321975275429689,0.333333333333333,0.321975275429689,0.333333333333333,
0.321975275429689,0.333333333333333,0.321975275429689,0.333333333333333,
0.321975275429689,0.333333333333333,0.321975275429689,0.333333333333333,
0.321975275429689,0.333333333333333,0.321975275429689,0.333333333333333,
0.321975275429689,0.333333333333333,0.321975275429689,0.333333333333333,
0.321975275429689,0.333333333333333,0.321975275429689,0.333333333333333,
0.321975275429689,0.333333333333333,0.321975275429689,0.333333333333333,
0.321975275429689,0.333333333333333,0.321975275429689,0.333333333333333,
0.321975275429689,0.333333333333333,0.321975275429689,0.333333333333333,
0.321975275429689,0.333333333333333,0.321975275429689,0.333333333333333,
0.321975275429689,0.333333333333333,0.321975275429689,0.333333333333333,
0.321975275429689,0.333333333333333,0.321975275429689,0.333333333333333,
0.321975275429689,0.333333333333333,0.321975275429689,0.333333333333333,
0.321975275429689,0.333333333333333,0.321975275429689,0.333333333333333,
0.321975275429689,0.333333333333333,0.321975275429689,0.333333333333333,
0.321975275429689,0.333333333333333,0.321975275429689,0.333333333333333,
0.321975275429689,0.333333333333333,0.321975275429689,0.333333333333333,
0.321975275429689,0.333333333333333,0.321975275429689,0.333333333333333,
0.321975275429689,0.333333333333333,0.321975275429689,0.333333333333333,
0.321975275429689,0.333333333333333,0.321975275429689,0.333333333333333,
0.321975275429689,0.333333333333333,0.321975275429689,0.333333333333333,
0.321975275429689,0.333333333333333),(1.,0.965925826289068,1.,0.965925826289068,
1.,0.965925826289068,1.,0.965925826289068,1.,0.965925826289068,1.,0.965925826289068,
1.,0.965925826289068,1.,0.965925826289068,1.,0.965925826289068,1.,0.965925826289068,
1.,0.965925826289068,1.,0.965925826289068,1.,0.965925826289068,1.,0.965925826289068,
1.,0.965925826289068,1.,0.965925826289068,1.,0.965925826289068,1.,0.965925826289068,
1.,0.965925826289068,1.,0.965925826289068,1.,0.965925826289068,1.,0.965925826289068,
1.,0.965925826289068,1.,0.965925826289068,1.,0.965925826289068,1.,0.965925826289068,
1.,0.965925826289068,1.,0.965925826289068,1.,0.965925826289068,1.,0.965925826289068,
1.,0.965925826289068,1.,0.965925826289068,1.,0.965925826289068,1.,0.965925826289068,
1.,0.965925826289068,1.,0.965925826289068,1.,0.965925826289068,1.,0.965925826289068,
1.,0.965925826289068,1.,0.965925826289068,1.,0.965925826289068,1.,0.965925826289068,
1.,0.965925826289068,1.,0.965925826289068,1.,0.965925826289068,1.,0.965925826289068,
1.,0.965925826289068,1.,0.965925826289068,1.,0.965925826289068,1.,0.965925826289068,
1.,0.965925826289068,1.,0.965925826289068,1.,0.965925826289068,1.,0.965925826289068,
1.,0.965925826289068,1.,0.965925826289068,1.,0.965925826289068,1.,0.965925826289068,
1.,0.965925826289068,1.,0.965925826289068,1.,0.965925826289068,1.,0.965925826289068,
1.,0.965925826289068,1.,0.965925826289068,1.,0.965925826289068,1.,0.965925826289068,
1.,0.965925826289068,1.,0.965925826289068,1.,0.965925826289068,1.,0.965925826289068,
1.,0.965925826289068,1.,0.965925826289068,1.,0.965925826289068,1.,0.965925826289068,
1.,0.965925826289068,1.,0.965925826289068,1.,0.965925826289068,1.,0.965925826289068,
1.,0.965925826289068,1.,0.965925826289068,1.,0.965925826289068,1.,0.965925826289068,
1.,0.965925826289068,1.,0.965925826289068,1.,0.965925826289068,1.,0.965925826289068,
1.,0.965925826289068,1.,0.965925826289068,1.,0.965925826289068,1.,0.965925826289068,
1.,0.965925826289068,1.,0.965925826289068,1.,0.965925826289068,1.,0.965925826289068,
1.,0.965925826289068,1.,0.965925826289068,1.,0.965925826289068,1.,0.965925826289068,
1.,0.965925826289068,1.,0.965925826289068,1.,0.965925826289068,1.,0.965925826289068,
1.,0.965925826289068,1.,0.965925826289068,1.,0.965925826289068,1.,0.965925826289068,
1.,0.965925826289068,1.,0.965925826289068,1.,0.965925826289068,1.,0.965925826289068,
1.,0.965925826289068,1.,0.965925826289068,1.,0.965925826289068,1.,0.965925826289068,
1.,0.965925826289068,1.,0.965925826289068,1.,0.965925826289068,1.,0.965925826289068,
1.,0.965925826289068,1.,0.965925826289068,1.)))
REPRESENTATION_ITEM('')
SURFACE()
);
#64=(
BOUNDED_SURFACE()
B_SPLINE_SURFACE(3,2,((#11567,#11568,#11569,#11570,#11571,#11572,#11573,
#11574,#11575,#11576,#11577,#11578,#11579,#11580,#11581,#11582,#11583,#11584,
#11585,#11586,#11587,#11588,#11589,#11590,#11591,#11592,#11593,#11594,#11595,
#11596,#11597,#11598,#11599,#11600,#11601,#11602,#11603,#11604,#11605,#11606,
#11607,#11608,#11609,#11610,#11611,#11612,#11613,#11614,#11615,#11616,#11617,
#11618,#11619,#11620,#11621,#11622,#11623,#11624,#11625,#11626,#11627,#11628,
#11629,#11630,#11631,#11632,#11633,#11634,#11635,#11636,#11637,#11638,#11639,
#11640,#11641,#11642,#11643,#11644,#11645,#11646,#11647,#11648,#11649,#11650,
#11651,#11652,#11653,#11654,#11655,#11656,#11657,#11658,#11659,#11660,#11661,
#11662,#11663,#11664,#11665,#11666,#11667,#11668,#11669,#11670,#11671,#11672,
#11673,#11674,#11675,#11676,#11677,#11678,#11679,#11680,#11681,#11682,#11683,
#11684,#11685,#11686,#11687,#11688,#11689,#11690,#11691,#11692,#11693,#11694,
#11695,#11696,#11697,#11698,#11699,#11700,#11701,#11702,#11703,#11704,#11705,
#11706,#11707,#11708,#11709,#11710,#11711,#11712,#11713,#11714,#11715,#11716,
#11717,#11718,#11719,#11720,#11721,#11722,#11723,#11724,#11725,#11726,#11727,
#11728,#11729,#11730,#11731,#11732,#11733,#11734,#11735,#11736,#11737,#11738,
#11739,#11740,#11741,#11742,#11743,#11744,#11745,#11746,#11747,#11748,#11749,
#11750,#11751,#11752,#11753,#11754,#11755,#11756,#11757,#11758,#11759,#11760,
#11761,#11762,#11763,#11764,#11765,#11766,#11767,#11768,#11769,#11770,#11771,
#11772,#11773,#11774,#11775,#11776,#11777,#11778,#11779,#11780,#11781,#11782,
#11783,#11784,#11785,#11786,#11787,#11788,#11789,#11790,#11791,#11792,#11793,
#11794,#11795,#11796,#11797,#11798,#11799,#11800,#11801,#11802,#11803,#11804,
#11805,#11806,#11807),(#11808,#11809,#11810,#11811,#11812,#11813,#11814,
#11815,#11816,#11817,#11818,#11819,#11820,#11821,#11822,#11823,#11824,#11825,
#11826,#11827,#11828,#11829,#11830,#11831,#11832,#11833,#11834,#11835,#11836,
#11837,#11838,#11839,#11840,#11841,#11842,#11843,#11844,#11845,#11846,#11847,
#11848,#11849,#11850,#11851,#11852,#11853,#11854,#11855,#11856,#11857,#11858,
#11859,#11860,#11861,#11862,#11863,#11864,#11865,#11866,#11867,#11868,#11869,
#11870,#11871,#11872,#11873,#11874,#11875,#11876,#11877,#11878,#11879,#11880,
#11881,#11882,#11883,#11884,#11885,#11886,#11887,#11888,#11889,#11890,#11891,
#11892,#11893,#11894,#11895,#11896,#11897,#11898,#11899,#11900,#11901,#11902,
#11903,#11904,#11905,#11906,#11907,#11908,#11909,#11910,#11911,#11912,#11913,
#11914,#11915,#11916,#11917,#11918,#11919,#11920,#11921,#11922,#11923,#11924,
#11925,#11926,#11927,#11928,#11929,#11930,#11931,#11932,#11933,#11934,#11935,
#11936,#11937,#11938,#11939,#11940,#11941,#11942,#11943,#11944,#11945,#11946,
#11947,#11948,#11949,#11950,#11951,#11952,#11953,#11954,#11955,#11956,#11957,
#11958,#11959,#11960,#11961,#11962,#11963,#11964,#11965,#11966,#11967,#11968,
#11969,#11970,#11971,#11972,#11973,#11974,#11975,#11976,#11977,#11978,#11979,
#11980,#11981,#11982,#11983,#11984,#11985,#11986,#11987,#11988,#11989,#11990,
#11991,#11992,#11993,#11994,#11995,#11996,#11997,#11998,#11999,#12000,#12001,
#12002,#12003,#12004,#12005,#12006,#12007,#12008,#12009,#12010,#12011,#12012,
#12013,#12014,#12015,#12016,#12017,#12018,#12019,#12020,#12021,#12022,#12023,
#12024,#12025,#12026,#12027,#12028,#12029,#12030,#12031,#12032,#12033,#12034,
#12035,#12036,#12037,#12038,#12039,#12040,#12041,#12042,#12043,#12044,#12045,
#12046,#12047,#12048),(#12049,#12050,#12051,#12052,#12053,#12054,#12055,
#12056,#12057,#12058,#12059,#12060,#12061,#12062,#12063,#12064,#12065,#12066,
#12067,#12068,#12069,#12070,#12071,#12072,#12073,#12074,#12075,#12076,#12077,
#12078,#12079,#12080,#12081,#12082,#12083,#12084,#12085,#12086,#12087,#12088,
#12089,#12090,#12091,#12092,#12093,#12094,#12095,#12096,#12097,#12098,#12099,
#12100,#12101,#12102,#12103,#12104,#12105,#12106,#12107,#12108,#12109,#12110,
#12111,#12112,#12113,#12114,#12115,#12116,#12117,#12118,#12119,#12120,#12121,
#12122,#12123,#12124,#12125,#12126,#12127,#12128,#12129,#12130,#12131,#12132,
#12133,#12134,#12135,#12136,#12137,#12138,#12139,#12140,#12141,#12142,#12143,
#12144,#12145,#12146,#12147,#12148,#12149,#12150,#12151,#12152,#12153,#12154,
#12155,#12156,#12157,#12158,#12159,#12160,#12161,#12162,#12163,#12164,#12165,
#12166,#12167,#12168,#12169,#12170,#12171,#12172,#12173,#12174,#12175,#12176,
#12177,#12178,#12179,#12180,#12181,#12182,#12183,#12184,#12185,#12186,#12187,
#12188,#12189,#12190,#12191,#12192,#12193,#12194,#12195,#12196,#12197,#12198,
#12199,#12200,#12201,#12202,#12203,#12204,#12205,#12206,#12207,#12208,#12209,
#12210,#12211,#12212,#12213,#12214,#12215,#12216,#12217,#12218,#12219,#12220,
#12221,#12222,#12223,#12224,#12225,#12226,#12227,#12228,#12229,#12230,#12231,
#12232,#12233,#12234,#12235,#12236,#12237,#12238,#12239,#12240,#12241,#12242,
#12243,#12244,#12245,#12246,#12247,#12248,#12249,#12250,#12251,#12252,#12253,
#12254,#12255,#12256,#12257,#12258,#12259,#12260,#12261,#12262,#12263,#12264,
#12265,#12266,#12267,#12268,#12269,#12270,#12271,#12272,#12273,#12274,#12275,
#12276,#12277,#12278,#12279,#12280,#12281,#12282,#12283,#12284,#12285,#12286,
#12287,#12288,#12289),(#12290,#12291,#12292,#12293,#12294,#12295,#12296,
#12297,#12298,#12299,#12300,#12301,#12302,#12303,#12304,#12305,#12306,#12307,
#12308,#12309,#12310,#12311,#12312,#12313,#12314,#12315,#12316,#12317,#12318,
#12319,#12320,#12321,#12322,#12323,#12324,#12325,#12326,#12327,#12328,#12329,
#12330,#12331,#12332,#12333,#12334,#12335,#12336,#12337,#12338,#12339,#12340,
#12341,#12342,#12343,#12344,#12345,#12346,#12347,#12348,#12349,#12350,#12351,
#12352,#12353,#12354,#12355,#12356,#12357,#12358,#12359,#12360,#12361,#12362,
#12363,#12364,#12365,#12366,#12367,#12368,#12369,#12370,#12371,#12372,#12373,
#12374,#12375,#12376,#12377,#12378,#12379,#12380,#12381,#12382,#12383,#12384,
#12385,#12386,#12387,#12388,#12389,#12390,#12391,#12392,#12393,#12394,#12395,
#12396,#12397,#12398,#12399,#12400,#12401,#12402,#12403,#12404,#12405,#12406,
#12407,#12408,#12409,#12410,#12411,#12412,#12413,#12414,#12415,#12416,#12417,
#12418,#12419,#12420,#12421,#12422,#12423,#12424,#12425,#12426,#12427,#12428,
#12429,#12430,#12431,#12432,#12433,#12434,#12435,#12436,#12437,#12438,#12439,
#12440,#12441,#12442,#12443,#12444,#12445,#12446,#12447,#12448,#12449,#12450,
#12451,#12452,#12453,#12454,#12455,#12456,#12457,#12458,#12459,#12460,#12461,
#12462,#12463,#12464,#12465,#12466,#12467,#12468,#12469,#12470,#12471,#12472,
#12473,#12474,#12475,#12476,#12477,#12478,#12479,#12480,#12481,#12482,#12483,
#12484,#12485,#12486,#12487,#12488,#12489,#12490,#12491,#12492,#12493,#12494,
#12495,#12496,#12497,#12498,#12499,#12500,#12501,#12502,#12503,#12504,#12505,
#12506,#12507,#12508,#12509,#12510,#12511,#12512,#12513,#12514,#12515,#12516,
#12517,#12518,#12519,#12520,#12521,#12522,#12523,#12524,#12525,#12526,#12527,
#12528,#12529,#12530),(#12531,#12532,#12533,#12534,#12535,#12536,#12537,
#12538,#12539,#12540,#12541,#12542,#12543,#12544,#12545,#12546,#12547,#12548,
#12549,#12550,#12551,#12552,#12553,#12554,#12555,#12556,#12557,#12558,#12559,
#12560,#12561,#12562,#12563,#12564,#12565,#12566,#12567,#12568,#12569,#12570,
#12571,#12572,#12573,#12574,#12575,#12576,#12577,#12578,#12579,#12580,#12581,
#12582,#12583,#12584,#12585,#12586,#12587,#12588,#12589,#12590,#12591,#12592,
#12593,#12594,#12595,#12596,#12597,#12598,#12599,#12600,#12601,#12602,#12603,
#12604,#12605,#12606,#12607,#12608,#12609,#12610,#12611,#12612,#12613,#12614,
#12615,#12616,#12617,#12618,#12619,#12620,#12621,#12622,#12623,#12624,#12625,
#12626,#12627,#12628,#12629,#12630,#12631,#12632,#12633,#12634,#12635,#12636,
#12637,#12638,#12639,#12640,#12641,#12642,#12643,#12644,#12645,#12646,#12647,
#12648,#12649,#12650,#12651,#12652,#12653,#12654,#12655,#12656,#12657,#12658,
#12659,#12660,#12661,#12662,#12663,#12664,#12665,#12666,#12667,#12668,#12669,
#12670,#12671,#12672,#12673,#12674,#12675,#12676,#12677,#12678,#12679,#12680,
#12681,#12682,#12683,#12684,#12685,#12686,#12687,#12688,#12689,#12690,#12691,
#12692,#12693,#12694,#12695,#12696,#12697,#12698,#12699,#12700,#12701,#12702,
#12703,#12704,#12705,#12706,#12707,#12708,#12709,#12710,#12711,#12712,#12713,
#12714,#12715,#12716,#12717,#12718,#12719,#12720,#12721,#12722,#12723,#12724,
#12725,#12726,#12727,#12728,#12729,#12730,#12731,#12732,#12733,#12734,#12735,
#12736,#12737,#12738,#12739,#12740,#12741,#12742,#12743,#12744,#12745,#12746,
#12747,#12748,#12749,#12750,#12751,#12752,#12753,#12754,#12755,#12756,#12757,
#12758,#12759,#12760,#12761,#12762,#12763,#12764,#12765,#12766,#12767,#12768,
#12769,#12770,#12771),(#12772,#12773,#12774,#12775,#12776,#12777,#12778,
#12779,#12780,#12781,#12782,#12783,#12784,#12785,#12786,#12787,#12788,#12789,
#12790,#12791,#12792,#12793,#12794,#12795,#12796,#12797,#12798,#12799,#12800,
#12801,#12802,#12803,#12804,#12805,#12806,#12807,#12808,#12809,#12810,#12811,
#12812,#12813,#12814,#12815,#12816,#12817,#12818,#12819,#12820,#12821,#12822,
#12823,#12824,#12825,#12826,#12827,#12828,#12829,#12830,#12831,#12832,#12833,
#12834,#12835,#12836,#12837,#12838,#12839,#12840,#12841,#12842,#12843,#12844,
#12845,#12846,#12847,#12848,#12849,#12850,#12851,#12852,#12853,#12854,#12855,
#12856,#12857,#12858,#12859,#12860,#12861,#12862,#12863,#12864,#12865,#12866,
#12867,#12868,#12869,#12870,#12871,#12872,#12873,#12874,#12875,#12876,#12877,
#12878,#12879,#12880,#12881,#12882,#12883,#12884,#12885,#12886,#12887,#12888,
#12889,#12890,#12891,#12892,#12893,#12894,#12895,#12896,#12897,#12898,#12899,
#12900,#12901,#12902,#12903,#12904,#12905,#12906,#12907,#12908,#12909,#12910,
#12911,#12912,#12913,#12914,#12915,#12916,#12917,#12918,#12919,#12920,#12921,
#12922,#12923,#12924,#12925,#12926,#12927,#12928,#12929,#12930,#12931,#12932,
#12933,#12934,#12935,#12936,#12937,#12938,#12939,#12940,#12941,#12942,#12943,
#12944,#12945,#12946,#12947,#12948,#12949,#12950,#12951,#12952,#12953,#12954,
#12955,#12956,#12957,#12958,#12959,#12960,#12961,#12962,#12963,#12964,#12965,
#12966,#12967,#12968,#12969,#12970,#12971,#12972,#12973,#12974,#12975,#12976,
#12977,#12978,#12979,#12980,#12981,#12982,#12983,#12984,#12985,#12986,#12987,
#12988,#12989,#12990,#12991,#12992,#12993,#12994,#12995,#12996,#12997,#12998,
#12999,#13000,#13001,#13002,#13003,#13004,#13005,#13006,#13007,#13008,#13009,
#13010,#13011,#13012),(#13013,#13014,#13015,#13016,#13017,#13018,#13019,
#13020,#13021,#13022,#13023,#13024,#13025,#13026,#13027,#13028,#13029,#13030,
#13031,#13032,#13033,#13034,#13035,#13036,#13037,#13038,#13039,#13040,#13041,
#13042,#13043,#13044,#13045,#13046,#13047,#13048,#13049,#13050,#13051,#13052,
#13053,#13054,#13055,#13056,#13057,#13058,#13059,#13060,#13061,#13062,#13063,
#13064,#13065,#13066,#13067,#13068,#13069,#13070,#13071,#13072,#13073,#13074,
#13075,#13076,#13077,#13078,#13079,#13080,#13081,#13082,#13083,#13084,#13085,
#13086,#13087,#13088,#13089,#13090,#13091,#13092,#13093,#13094,#13095,#13096,
#13097,#13098,#13099,#13100,#13101,#13102,#13103,#13104,#13105,#13106,#13107,
#13108,#13109,#13110,#13111,#13112,#13113,#13114,#13115,#13116,#13117,#13118,
#13119,#13120,#13121,#13122,#13123,#13124,#13125,#13126,#13127,#13128,#13129,
#13130,#13131,#13132,#13133,#13134,#13135,#13136,#13137,#13138,#13139,#13140,
#13141,#13142,#13143,#13144,#13145,#13146,#13147,#13148,#13149,#13150,#13151,
#13152,#13153,#13154,#13155,#13156,#13157,#13158,#13159,#13160,#13161,#13162,
#13163,#13164,#13165,#13166,#13167,#13168,#13169,#13170,#13171,#13172,#13173,
#13174,#13175,#13176,#13177,#13178,#13179,#13180,#13181,#13182,#13183,#13184,
#13185,#13186,#13187,#13188,#13189,#13190,#13191,#13192,#13193,#13194,#13195,
#13196,#13197,#13198,#13199,#13200,#13201,#13202,#13203,#13204,#13205,#13206,
#13207,#13208,#13209,#13210,#13211,#13212,#13213,#13214,#13215,#13216,#13217,
#13218,#13219,#13220,#13221,#13222,#13223,#13224,#13225,#13226,#13227,#13228,
#13229,#13230,#13231,#13232,#13233,#13234,#13235,#13236,#13237,#13238,#13239,
#13240,#13241,#13242,#13243,#13244,#13245,#13246,#13247,#13248,#13249,#13250,
#13251,#13252,#13253)),.UNSPECIFIED.,.T.,.F.,.F.)
B_SPLINE_SURFACE_WITH_KNOTS((4,3,4),(3,2,2,2,2,2,2,2,2,2,2,2,2,2,2,2,2,
2,2,2,2,2,2,2,2,2,2,2,2,2,2,2,2,2,2,2,2,2,2,2,2,2,2,2,2,2,2,2,2,2,2,2,2,
2,2,2,2,2,2,2,2,2,2,2,2,2,2,2,2,2,2,2,2,2,2,2,2,2,2,2,2,2,2,2,2,2,2,2,2,
2,2,2,2,2,2,2,2,2,2,2,2,2,2,2,2,2,2,2,2,2,2,2,2,2,2,2,2,2,2,2,3),(0.,0.5,
1.),(0.,0.00833333333333333,0.0166666666666667,0.025,0.0333333333333333,
0.0416666666666667,0.05,0.0583333333333333,0.0666666666666667,0.075,0.0833333333333333,
0.0916666666666667,0.1,0.108333333333333,0.116666666666667,0.125,0.133333333333333,
0.141666666666667,0.15,0.158333333333333,0.166666666666667,0.175,0.183333333333333,
0.191666666666667,0.2,0.208333333333333,0.216666666666667,0.225,0.233333333333333,
0.241666666666667,0.25,0.258333333333333,0.266666666666667,0.275,0.283333333333333,
0.291666666666667,0.3,0.308333333333333,0.316666666666667,0.325,0.333333333333333,
0.341666666666667,0.35,0.358333333333333,0.366666666666667,0.375,0.383333333333333,
0.391666666666667,0.4,0.408333333333333,0.416666666666667,0.425,0.433333333333333,
0.441666666666667,0.45,0.458333333333333,0.466666666666667,0.475,0.483333333333333,
0.491666666666667,0.5,0.508333333333333,0.516666666666667,0.525,0.533333333333333,
0.541666666666667,0.55,0.558333333333333,0.566666666666667,0.575,0.583333333333333,
0.591666666666667,0.6,0.608333333333333,0.616666666666667,0.625,0.633333333333333,
0.641666666666667,0.65,0.658333333333333,0.666666666666667,0.675,0.683333333333333,
0.691666666666667,0.7,0.708333333333333,0.716666666666667,0.725,0.733333333333333,
0.741666666666667,0.75,0.758333333333333,0.766666666666667,0.775,0.783333333333333,
0.791666666666667,0.8,0.808333333333333,0.816666666666667,0.825,0.833333333333333,
0.841666666666667,0.85,0.858333333333333,0.866666666666667,0.875,0.883333333333333,
0.891666666666667,0.9,0.908333333333333,0.916666666666667,0.925,0.933333333333333,
0.941666666666667,0.95,0.958333333333333,0.966666666666667,0.975,0.983333333333333,
0.991666666666667,1.),.UNSPECIFIED.)
GEOMETRIC_REPRESENTATION_ITEM()
RATIONAL_B_SPLINE_SURFACE(((1.,0.965925826289068,1.,0.965925826289068,1.,
0.965925826289068,1.,0.965925826289068,1.,0.965925826289068,1.,0.965925826289068,
1.,0.965925826289068,1.,0.965925826289068,1.,0.965925826289068,1.,0.965925826289068,
1.,0.965925826289068,1.,0.965925826289068,1.,0.965925826289068,1.,0.965925826289068,
1.,0.965925826289068,1.,0.965925826289068,1.,0.965925826289068,1.,0.965925826289068,
1.,0.965925826289068,1.,0.965925826289068,1.,0.965925826289068,1.,0.965925826289068,
1.,0.965925826289068,1.,0.965925826289068,1.,0.965925826289068,1.,0.965925826289068,
1.,0.965925826289068,1.,0.965925826289068,1.,0.965925826289068,1.,0.965925826289068,
1.,0.965925826289068,1.,0.965925826289068,1.,0.965925826289068,1.,0.965925826289068,
1.,0.965925826289068,1.,0.965925826289068,1.,0.965925826289068,1.,0.965925826289068,
1.,0.965925826289068,1.,0.965925826289068,1.,0.965925826289068,1.,0.965925826289068,
1.,0.965925826289068,1.,0.965925826289068,1.,0.965925826289068,1.,0.965925826289068,
1.,0.965925826289068,1.,0.965925826289068,1.,0.965925826289068,1.,0.965925826289068,
1.,0.965925826289068,1.,0.965925826289068,1.,0.965925826289068,1.,0.965925826289068,
1.,0.965925826289068,1.,0.965925826289068,1.,0.965925826289068,1.,0.965925826289068,
1.,0.965925826289068,1.,0.965925826289068,1.,0.965925826289068,1.,0.965925826289068,
1.,0.965925826289068,1.,0.965925826289068,1.,0.965925826289068,1.,0.965925826289068,
1.,0.965925826289068,1.,0.965925826289068,1.,0.965925826289068,1.,0.965925826289068,
1.,0.965925826289068,1.,0.965925826289068,1.,0.965925826289068,1.,0.965925826289068,
1.,0.965925826289068,1.,0.965925826289068,1.,0.965925826289068,1.,0.965925826289068,
1.,0.965925826289068,1.,0.965925826289068,1.,0.965925826289068,1.,0.965925826289068,
1.,0.965925826289068,1.,0.965925826289068,1.,0.965925826289068,1.,0.965925826289068,
1.,0.965925826289068,1.,0.965925826289068,1.,0.965925826289068,1.,0.965925826289068,
1.,0.965925826289068,1.,0.965925826289068,1.,0.965925826289068,1.,0.965925826289068,
1.,0.965925826289068,1.,0.965925826289068,1.,0.965925826289068,1.,0.965925826289068,
1.,0.965925826289068,1.,0.965925826289068,1.,0.965925826289068,1.,0.965925826289068,
1.,0.965925826289068,1.,0.965925826289068,1.,0.965925826289068,1.,0.965925826289068,
1.,0.965925826289068,1.,0.965925826289068,1.,0.965925826289068,1.,0.965925826289068,
1.,0.965925826289068,1.,0.965925826289068,1.,0.965925826289068,1.,0.965925826289068,
1.,0.965925826289068,1.,0.965925826289068,1.,0.965925826289068,1.,0.965925826289068,
1.,0.965925826289068,1.,0.965925826289068,1.),(0.333333333333333,0.321975275429689,
0.333333333333333,0.321975275429689,0.333333333333333,0.321975275429689,
0.333333333333333,0.321975275429689,0.333333333333333,0.321975275429689,
0.333333333333333,0.321975275429689,0.333333333333333,0.321975275429689,
0.333333333333333,0.321975275429689,0.333333333333333,0.321975275429689,
0.333333333333333,0.321975275429689,0.333333333333333,0.321975275429689,
0.333333333333333,0.321975275429689,0.333333333333333,0.321975275429689,
0.333333333333333,0.321975275429689,0.333333333333333,0.321975275429689,
0.333333333333333,0.321975275429689,0.333333333333333,0.321975275429689,
0.333333333333333,0.321975275429689,0.333333333333333,0.321975275429689,
0.333333333333333,0.321975275429689,0.333333333333333,0.321975275429689,
0.333333333333333,0.321975275429689,0.333333333333333,0.321975275429689,
0.333333333333333,0.321975275429689,0.333333333333333,0.321975275429689,
0.333333333333333,0.321975275429689,0.333333333333333,0.321975275429689,
0.333333333333333,0.321975275429689,0.333333333333333,0.321975275429689,
0.333333333333333,0.321975275429689,0.333333333333333,0.321975275429689,
0.333333333333333,0.321975275429689,0.333333333333333,0.321975275429689,
0.333333333333333,0.321975275429689,0.333333333333333,0.321975275429689,
0.333333333333333,0.321975275429689,0.333333333333333,0.321975275429689,
0.333333333333333,0.321975275429689,0.333333333333333,0.321975275429689,
0.333333333333333,0.321975275429689,0.333333333333333,0.321975275429689,
0.333333333333333,0.321975275429689,0.333333333333333,0.321975275429689,
0.333333333333333,0.321975275429689,0.333333333333333,0.321975275429689,
0.333333333333333,0.321975275429689,0.333333333333333,0.321975275429689,
0.333333333333333,0.321975275429689,0.333333333333333,0.321975275429689,
0.333333333333333,0.321975275429689,0.333333333333333,0.321975275429689,
0.333333333333333,0.321975275429689,0.333333333333333,0.321975275429689,
0.333333333333333,0.321975275429689,0.333333333333333,0.321975275429689,
0.333333333333333,0.321975275429689,0.333333333333333,0.321975275429689,
0.333333333333333,0.321975275429689,0.333333333333333,0.321975275429689,
0.333333333333333,0.321975275429689,0.333333333333333,0.321975275429689,
0.333333333333333,0.321975275429689,0.333333333333333,0.321975275429689,
0.333333333333333,0.321975275429689,0.333333333333333,0.321975275429689,
0.333333333333333,0.321975275429689,0.333333333333333,0.321975275429689,
0.333333333333333,0.321975275429689,0.333333333333333,0.321975275429689,
0.333333333333333,0.321975275429689,0.333333333333333,0.321975275429689,
0.333333333333333,0.321975275429689,0.333333333333333,0.321975275429689,
0.333333333333333,0.321975275429689,0.333333333333333,0.321975275429689,
0.333333333333333,0.321975275429689,0.333333333333333,0.321975275429689,
0.333333333333333,0.321975275429689,0.333333333333333,0.321975275429689,
0.333333333333333,0.321975275429689,0.333333333333333,0.321975275429689,
0.333333333333333,0.321975275429689,0.333333333333333,0.321975275429689,
0.333333333333333,0.321975275429689,0.333333333333333,0.321975275429689,
0.333333333333333,0.321975275429689,0.333333333333333,0.321975275429689,
0.333333333333333,0.321975275429689,0.333333333333333,0.321975275429689,
0.333333333333333,0.321975275429689,0.333333333333333,0.321975275429689,
0.333333333333333,0.321975275429689,0.333333333333333,0.321975275429689,
0.333333333333333,0.321975275429689,0.333333333333333,0.321975275429689,
0.333333333333333,0.321975275429689,0.333333333333333,0.321975275429689,
0.333333333333333,0.321975275429689,0.333333333333333,0.321975275429689,
0.333333333333333,0.321975275429689,0.333333333333333,0.321975275429689,
0.333333333333333,0.321975275429689,0.333333333333333,0.321975275429689,
0.333333333333333,0.321975275429689,0.333333333333333,0.321975275429689,
0.333333333333333,0.321975275429689,0.333333333333333,0.321975275429689,
0.333333333333333,0.321975275429689,0.333333333333333,0.321975275429689,
0.333333333333333,0.321975275429689,0.333333333333333,0.321975275429689,
0.333333333333333,0.321975275429689,0.333333333333333,0.321975275429689,
0.333333333333333,0.321975275429689,0.333333333333333,0.321975275429689,
0.333333333333333,0.321975275429689,0.333333333333333,0.321975275429689,
0.333333333333333,0.321975275429689,0.333333333333333,0.321975275429689,
0.333333333333333,0.321975275429689,0.333333333333333),(0.333333333333333,
0.321975275429689,0.333333333333333,0.321975275429689,0.333333333333333,
0.321975275429689,0.333333333333333,0.321975275429689,0.333333333333333,
0.321975275429689,0.333333333333333,0.321975275429689,0.333333333333333,
0.321975275429689,0.333333333333333,0.321975275429689,0.333333333333333,
0.321975275429689,0.333333333333333,0.321975275429689,0.333333333333333,
0.321975275429689,0.333333333333333,0.321975275429689,0.333333333333333,
0.321975275429689,0.333333333333333,0.321975275429689,0.333333333333333,
0.321975275429689,0.333333333333333,0.321975275429689,0.333333333333333,
0.321975275429689,0.333333333333333,0.321975275429689,0.333333333333333,
0.321975275429689,0.333333333333333,0.321975275429689,0.333333333333333,
0.321975275429689,0.333333333333333,0.321975275429689,0.333333333333333,
0.321975275429689,0.333333333333333,0.321975275429689,0.333333333333333,
0.321975275429689,0.333333333333333,0.321975275429689,0.333333333333333,
0.321975275429689,0.333333333333333,0.321975275429689,0.333333333333333,
0.321975275429689,0.333333333333333,0.321975275429689,0.333333333333333,
0.321975275429689,0.333333333333333,0.321975275429689,0.333333333333333,
0.321975275429689,0.333333333333333,0.321975275429689,0.333333333333333,
0.321975275429689,0.333333333333333,0.321975275429689,0.333333333333333,
0.321975275429689,0.333333333333333,0.321975275429689,0.333333333333333,
0.321975275429689,0.333333333333333,0.321975275429689,0.333333333333333,
0.321975275429689,0.333333333333333,0.321975275429689,0.333333333333333,
0.321975275429689,0.333333333333333,0.321975275429689,0.333333333333333,
0.321975275429689,0.333333333333333,0.321975275429689,0.333333333333333,
0.321975275429689,0.333333333333333,0.321975275429689,0.333333333333333,
0.321975275429689,0.333333333333333,0.321975275429689,0.333333333333333,
0.321975275429689,0.333333333333333,0.321975275429689,0.333333333333333,
0.321975275429689,0.333333333333333,0.321975275429689,0.333333333333333,
0.321975275429689,0.333333333333333,0.321975275429689,0.333333333333333,
0.321975275429689,0.333333333333333,0.321975275429689,0.333333333333333,
0.321975275429689,0.333333333333333,0.321975275429689,0.333333333333333,
0.321975275429689,0.333333333333333,0.321975275429689,0.333333333333333,
0.321975275429689,0.333333333333333,0.321975275429689,0.333333333333333,
0.321975275429689,0.333333333333333,0.321975275429689,0.333333333333333,
0.321975275429689,0.333333333333333,0.321975275429689,0.333333333333333,
0.321975275429689,0.333333333333333,0.321975275429689,0.333333333333333,
0.321975275429689,0.333333333333333,0.321975275429689,0.333333333333333,
0.321975275429689,0.333333333333333,0.321975275429689,0.333333333333333,
0.321975275429689,0.333333333333333,0.321975275429689,0.333333333333333,
0.321975275429689,0.333333333333333,0.321975275429689,0.333333333333333,
0.321975275429689,0.333333333333333,0.321975275429689,0.333333333333333,
0.321975275429689,0.333333333333333,0.321975275429689,0.333333333333333,
0.321975275429689,0.333333333333333,0.321975275429689,0.333333333333333,
0.321975275429689,0.333333333333333,0.321975275429689,0.333333333333333,
0.321975275429689,0.333333333333333,0.321975275429689,0.333333333333333,
0.321975275429689,0.333333333333333,0.321975275429689,0.333333333333333,
0.321975275429689,0.333333333333333,0.321975275429689,0.333333333333333,
0.321975275429689,0.333333333333333,0.321975275429689,0.333333333333333,
0.321975275429689,0.333333333333333,0.321975275429689,0.333333333333333,
0.321975275429689,0.333333333333333,0.321975275429689,0.333333333333333,
0.321975275429689,0.333333333333333,0.321975275429689,0.333333333333333,
0.321975275429689,0.333333333333333,0.321975275429689,0.333333333333333,
0.321975275429689,0.333333333333333,0.321975275429689,0.333333333333333,
0.321975275429689,0.333333333333333,0.321975275429689,0.333333333333333,
0.321975275429689,0.333333333333333,0.321975275429689,0.333333333333333,
0.321975275429689,0.333333333333333,0.321975275429689,0.333333333333333,
0.321975275429689,0.333333333333333,0.321975275429689,0.333333333333333,
0.321975275429689,0.333333333333333,0.321975275429689,0.333333333333333,
0.321975275429689,0.333333333333333,0.321975275429689,0.333333333333333,
0.321975275429689,0.333333333333333,0.321975275429689,0.333333333333333,
0.321975275429689,0.333333333333333,0.321975275429689,0.333333333333333),
(1.,0.965925826289068,1.,0.965925826289068,1.,0.965925826289068,1.,0.965925826289068,
1.,0.965925826289068,1.,0.965925826289068,1.,0.965925826289068,1.,0.965925826289068,
1.,0.965925826289068,1.,0.965925826289068,1.,0.965925826289068,1.,0.965925826289068,
1.,0.965925826289068,1.,0.965925826289068,1.,0.965925826289068,1.,0.965925826289068,
1.,0.965925826289068,1.,0.965925826289068,1.,0.965925826289068,1.,0.965925826289068,
1.,0.965925826289068,1.,0.965925826289068,1.,0.965925826289068,1.,0.965925826289068,
1.,0.965925826289068,1.,0.965925826289068,1.,0.965925826289068,1.,0.965925826289068,
1.,0.965925826289068,1.,0.965925826289068,1.,0.965925826289068,1.,0.965925826289068,
1.,0.965925826289068,1.,0.965925826289068,1.,0.965925826289068,1.,0.965925826289068,
1.,0.965925826289068,1.,0.965925826289068,1.,0.965925826289068,1.,0.965925826289068,
1.,0.965925826289068,1.,0.965925826289068,1.,0.965925826289068,1.,0.965925826289068,
1.,0.965925826289068,1.,0.965925826289068,1.,0.965925826289068,1.,0.965925826289068,
1.,0.965925826289068,1.,0.965925826289068,1.,0.965925826289068,1.,0.965925826289068,
1.,0.965925826289068,1.,0.965925826289068,1.,0.965925826289068,1.,0.965925826289068,
1.,0.965925826289068,1.,0.965925826289068,1.,0.965925826289068,1.,0.965925826289068,
1.,0.965925826289068,1.,0.965925826289068,1.,0.965925826289068,1.,0.965925826289068,
1.,0.965925826289068,1.,0.965925826289068,1.,0.965925826289068,1.,0.965925826289068,
1.,0.965925826289068,1.,0.965925826289068,1.,0.965925826289068,1.,0.965925826289068,
1.,0.965925826289068,1.,0.965925826289068,1.,0.965925826289068,1.,0.965925826289068,
1.,0.965925826289068,1.,0.965925826289068,1.,0.965925826289068,1.,0.965925826289068,
1.,0.965925826289068,1.,0.965925826289068,1.,0.965925826289068,1.,0.965925826289068,
1.,0.965925826289068,1.,0.965925826289068,1.,0.965925826289068,1.,0.965925826289068,
1.,0.965925826289068,1.,0.965925826289068,1.,0.965925826289068,1.,0.965925826289068,
1.,0.965925826289068,1.,0.965925826289068,1.,0.965925826289068,1.,0.965925826289068,
1.,0.965925826289068,1.,0.965925826289068,1.,0.965925826289068,1.,0.965925826289068,
1.,0.965925826289068,1.,0.965925826289068,1.,0.965925826289068,1.,0.965925826289068,
1.,0.965925826289068,1.,0.965925826289068,1.,0.965925826289068,1.,0.965925826289068,
1.,0.965925826289068,1.,0.965925826289068,1.,0.965925826289068,1.,0.965925826289068,
1.,0.965925826289068,1.,0.965925826289068,1.,0.965925826289068,1.,0.965925826289068,
1.,0.965925826289068,1.,0.965925826289068,1.,0.965925826289068,1.,0.965925826289068,
1.),(0.333333333333333,0.321975275429689,0.333333333333333,0.321975275429689,
0.333333333333333,0.321975275429689,0.333333333333333,0.321975275429689,
0.333333333333333,0.321975275429689,0.333333333333333,0.321975275429689,
0.333333333333333,0.321975275429689,0.333333333333333,0.321975275429689,
0.333333333333333,0.321975275429689,0.333333333333333,0.321975275429689,
0.333333333333333,0.321975275429689,0.333333333333333,0.321975275429689,
0.333333333333333,0.321975275429689,0.333333333333333,0.321975275429689,
0.333333333333333,0.321975275429689,0.333333333333333,0.321975275429689,
0.333333333333333,0.321975275429689,0.333333333333333,0.321975275429689,
0.333333333333333,0.321975275429689,0.333333333333333,0.321975275429689,
0.333333333333333,0.321975275429689,0.333333333333333,0.321975275429689,
0.333333333333333,0.321975275429689,0.333333333333333,0.321975275429689,
0.333333333333333,0.321975275429689,0.333333333333333,0.321975275429689,
0.333333333333333,0.321975275429689,0.333333333333333,0.321975275429689,
0.333333333333333,0.321975275429689,0.333333333333333,0.321975275429689,
0.333333333333333,0.321975275429689,0.333333333333333,0.321975275429689,
0.333333333333333,0.321975275429689,0.333333333333333,0.321975275429689,
0.333333333333333,0.321975275429689,0.333333333333333,0.321975275429689,
0.333333333333333,0.321975275429689,0.333333333333333,0.321975275429689,
0.333333333333333,0.321975275429689,0.333333333333333,0.321975275429689,
0.333333333333333,0.321975275429689,0.333333333333333,0.321975275429689,
0.333333333333333,0.321975275429689,0.333333333333333,0.321975275429689,
0.333333333333333,0.321975275429689,0.333333333333333,0.321975275429689,
0.333333333333333,0.321975275429689,0.333333333333333,0.321975275429689,
0.333333333333333,0.321975275429689,0.333333333333333,0.321975275429689,
0.333333333333333,0.321975275429689,0.333333333333333,0.321975275429689,
0.333333333333333,0.321975275429689,0.333333333333333,0.321975275429689,
0.333333333333333,0.321975275429689,0.333333333333333,0.321975275429689,
0.333333333333333,0.321975275429689,0.333333333333333,0.321975275429689,
0.333333333333333,0.321975275429689,0.333333333333333,0.321975275429689,
0.333333333333333,0.321975275429689,0.333333333333333,0.321975275429689,
0.333333333333333,0.321975275429689,0.333333333333333,0.321975275429689,
0.333333333333333,0.321975275429689,0.333333333333333,0.321975275429689,
0.333333333333333,0.321975275429689,0.333333333333333,0.321975275429689,
0.333333333333333,0.321975275429689,0.333333333333333,0.321975275429689,
0.333333333333333,0.321975275429689,0.333333333333333,0.321975275429689,
0.333333333333333,0.321975275429689,0.333333333333333,0.321975275429689,
0.333333333333333,0.321975275429689,0.333333333333333,0.321975275429689,
0.333333333333333,0.321975275429689,0.333333333333333,0.321975275429689,
0.333333333333333,0.321975275429689,0.333333333333333,0.321975275429689,
0.333333333333333,0.321975275429689,0.333333333333333,0.321975275429689,
0.333333333333333,0.321975275429689,0.333333333333333,0.321975275429689,
0.333333333333333,0.321975275429689,0.333333333333333,0.321975275429689,
0.333333333333333,0.321975275429689,0.333333333333333,0.321975275429689,
0.333333333333333,0.321975275429689,0.333333333333333,0.321975275429689,
0.333333333333333,0.321975275429689,0.333333333333333,0.321975275429689,
0.333333333333333,0.321975275429689,0.333333333333333,0.321975275429689,
0.333333333333333,0.321975275429689,0.333333333333333,0.321975275429689,
0.333333333333333,0.321975275429689,0.333333333333333,0.321975275429689,
0.333333333333333,0.321975275429689,0.333333333333333,0.321975275429689,
0.333333333333333,0.321975275429689,0.333333333333333,0.321975275429689,
0.333333333333333,0.321975275429689,0.333333333333333,0.321975275429689,
0.333333333333333,0.321975275429689,0.333333333333333,0.321975275429689,
0.333333333333333,0.321975275429689,0.333333333333333,0.321975275429689,
0.333333333333333,0.321975275429689,0.333333333333333,0.321975275429689,
0.333333333333333,0.321975275429689,0.333333333333333,0.321975275429689,
0.333333333333333,0.321975275429689,0.333333333333333,0.321975275429689,
0.333333333333333,0.321975275429689,0.333333333333333,0.321975275429689,
0.333333333333333,0.321975275429689,0.333333333333333,0.321975275429689,
0.333333333333333,0.321975275429689,0.333333333333333,0.321975275429689,
0.333333333333333),(0.333333333333333,0.321975275429689,0.333333333333333,
0.321975275429689,0.333333333333333,0.321975275429689,0.333333333333333,
0.321975275429689,0.333333333333333,0.321975275429689,0.333333333333333,
0.321975275429689,0.333333333333333,0.321975275429689,0.333333333333333,
0.321975275429689,0.333333333333333,0.321975275429689,0.333333333333333,
0.321975275429689,0.333333333333333,0.321975275429689,0.333333333333333,
0.321975275429689,0.333333333333333,0.321975275429689,0.333333333333333,
0.321975275429689,0.333333333333333,0.321975275429689,0.333333333333333,
0.321975275429689,0.333333333333333,0.321975275429689,0.333333333333333,
0.321975275429689,0.333333333333333,0.321975275429689,0.333333333333333,
0.321975275429689,0.333333333333333,0.321975275429689,0.333333333333333,
0.321975275429689,0.333333333333333,0.321975275429689,0.333333333333333,
0.321975275429689,0.333333333333333,0.321975275429689,0.333333333333333,
0.321975275429689,0.333333333333333,0.321975275429689,0.333333333333333,
0.321975275429689,0.333333333333333,0.321975275429689,0.333333333333333,
0.321975275429689,0.333333333333333,0.321975275429689,0.333333333333333,
0.321975275429689,0.333333333333333,0.321975275429689,0.333333333333333,
0.321975275429689,0.333333333333333,0.321975275429689,0.333333333333333,
0.321975275429689,0.333333333333333,0.321975275429689,0.333333333333333,
0.321975275429689,0.333333333333333,0.321975275429689,0.333333333333333,
0.321975275429689,0.333333333333333,0.321975275429689,0.333333333333333,
0.321975275429689,0.333333333333333,0.321975275429689,0.333333333333333,
0.321975275429689,0.333333333333333,0.321975275429689,0.333333333333333,
0.321975275429689,0.333333333333333,0.321975275429689,0.333333333333333,
0.321975275429689,0.333333333333333,0.321975275429689,0.333333333333333,
0.321975275429689,0.333333333333333,0.321975275429689,0.333333333333333,
0.321975275429689,0.333333333333333,0.321975275429689,0.333333333333333,
0.321975275429689,0.333333333333333,0.321975275429689,0.333333333333333,
0.321975275429689,0.333333333333333,0.321975275429689,0.333333333333333,
0.321975275429689,0.333333333333333,0.321975275429689,0.333333333333333,
0.321975275429689,0.333333333333333,0.321975275429689,0.333333333333333,
0.321975275429689,0.333333333333333,0.321975275429689,0.333333333333333,
0.321975275429689,0.333333333333333,0.321975275429689,0.333333333333333,
0.321975275429689,0.333333333333333,0.321975275429689,0.333333333333333,
0.321975275429689,0.333333333333333,0.321975275429689,0.333333333333333,
0.321975275429689,0.333333333333333,0.321975275429689,0.333333333333333,
0.321975275429689,0.333333333333333,0.321975275429689,0.333333333333333,
0.321975275429689,0.333333333333333,0.321975275429689,0.333333333333333,
0.321975275429689,0.333333333333333,0.321975275429689,0.333333333333333,
0.321975275429689,0.333333333333333,0.321975275429689,0.333333333333333,
0.321975275429689,0.333333333333333,0.321975275429689,0.333333333333333,
0.321975275429689,0.333333333333333,0.321975275429689,0.333333333333333,
0.321975275429689,0.333333333333333,0.321975275429689,0.333333333333333,
0.321975275429689,0.333333333333333,0.321975275429689,0.333333333333333,
0.321975275429689,0.333333333333333,0.321975275429689,0.333333333333333,
0.321975275429689,0.333333333333333,0.321975275429689,0.333333333333333,
0.321975275429689,0.333333333333333,0.321975275429689,0.333333333333333,
0.321975275429689,0.333333333333333,0.321975275429689,0.333333333333333,
0.321975275429689,0.333333333333333,0.321975275429689,0.333333333333333,
0.321975275429689,0.333333333333333,0.321975275429689,0.333333333333333,
0.321975275429689,0.333333333333333,0.321975275429689,0.333333333333333,
0.321975275429689,0.333333333333333,0.321975275429689,0.333333333333333,
0.321975275429689,0.333333333333333,0.321975275429689,0.333333333333333,
0.321975275429689,0.333333333333333,0.321975275429689,0.333333333333333,
0.321975275429689,0.333333333333333,0.321975275429689,0.333333333333333,
0.321975275429689,0.333333333333333,0.321975275429689,0.333333333333333,
0.321975275429689,0.333333333333333,0.321975275429689,0.333333333333333,
0.321975275429689,0.333333333333333,0.321975275429689,0.333333333333333,
0.321975275429689,0.333333333333333,0.321975275429689,0.333333333333333,
0.321975275429689,0.333333333333333,0.321975275429689,0.333333333333333,
0.321975275429689,0.333333333333333),(1.,0.965925826289068,1.,0.965925826289068,
1.,0.965925826289068,1.,0.965925826289068,1.,0.965925826289068,1.,0.965925826289068,
1.,0.965925826289068,1.,0.965925826289068,1.,0.965925826289068,1.,0.965925826289068,
1.,0.965925826289068,1.,0.965925826289068,1.,0.965925826289068,1.,0.965925826289068,
1.,0.965925826289068,1.,0.965925826289068,1.,0.965925826289068,1.,0.965925826289068,
1.,0.965925826289068,1.,0.965925826289068,1.,0.965925826289068,1.,0.965925826289068,
1.,0.965925826289068,1.,0.965925826289068,1.,0.965925826289068,1.,0.965925826289068,
1.,0.965925826289068,1.,0.965925826289068,1.,0.965925826289068,1.,0.965925826289068,
1.,0.965925826289068,1.,0.965925826289068,1.,0.965925826289068,1.,0.965925826289068,
1.,0.965925826289068,1.,0.965925826289068,1.,0.965925826289068,1.,0.965925826289068,
1.,0.965925826289068,1.,0.965925826289068,1.,0.965925826289068,1.,0.965925826289068,
1.,0.965925826289068,1.,0.965925826289068,1.,0.965925826289068,1.,0.965925826289068,
1.,0.965925826289068,1.,0.965925826289068,1.,0.965925826289068,1.,0.965925826289068,
1.,0.965925826289068,1.,0.965925826289068,1.,0.965925826289068,1.,0.965925826289068,
1.,0.965925826289068,1.,0.965925826289068,1.,0.965925826289068,1.,0.965925826289068,
1.,0.965925826289068,1.,0.965925826289068,1.,0.965925826289068,1.,0.965925826289068,
1.,0.965925826289068,1.,0.965925826289068,1.,0.965925826289068,1.,0.965925826289068,
1.,0.965925826289068,1.,0.965925826289068,1.,0.965925826289068,1.,0.965925826289068,
1.,0.965925826289068,1.,0.965925826289068,1.,0.965925826289068,1.,0.965925826289068,
1.,0.965925826289068,1.,0.965925826289068,1.,0.965925826289068,1.,0.965925826289068,
1.,0.965925826289068,1.,0.965925826289068,1.,0.965925826289068,1.,0.965925826289068,
1.,0.965925826289068,1.,0.965925826289068,1.,0.965925826289068,1.,0.965925826289068,
1.,0.965925826289068,1.,0.965925826289068,1.,0.965925826289068,1.,0.965925826289068,
1.,0.965925826289068,1.,0.965925826289068,1.,0.965925826289068,1.,0.965925826289068,
1.,0.965925826289068,1.,0.965925826289068,1.,0.965925826289068,1.,0.965925826289068,
1.,0.965925826289068,1.,0.965925826289068,1.,0.965925826289068,1.,0.965925826289068,
1.,0.965925826289068,1.,0.965925826289068,1.,0.965925826289068,1.,0.965925826289068,
1.,0.965925826289068,1.,0.965925826289068,1.,0.965925826289068,1.,0.965925826289068,
1.,0.965925826289068,1.,0.965925826289068,1.,0.965925826289068,1.,0.965925826289068,
1.,0.965925826289068,1.,0.965925826289068,1.,0.965925826289068,1.,0.965925826289068,
1.,0.965925826289068,1.,0.965925826289068,1.)))
REPRESENTATION_ITEM('')
SURFACE()
);
#65=(
BOUNDED_SURFACE()
B_SPLINE_SURFACE(3,2,((#13700,#13701,#13702),(#13703,#13704,#13705),(#13706,
#13707,#13708),(#13709,#13710,#13711),(#13712,#13713,#13714),(#13715,#13716,
#13717),(#13718,#13719,#13720),(#13721,#13722,#13723)),.UNSPECIFIED.,.F.,
 .F.,.F.)
B_SPLINE_SURFACE_WITH_KNOTS((4,2,2,4),(3,3),(0.0461385444250929,0.0516992567704878,
0.0544796129431853,0.0572599691158828),(0.,1.00002275764424),
 .UNSPECIFIED.)
GEOMETRIC_REPRESENTATION_ITEM()
RATIONAL_B_SPLINE_SURFACE(((1.,0.804773725708204,1.00000888578019),(1.,
0.812372242905555,1.00000853993149),(1.,0.819062000811371,1.00000823544523),
(1.,0.819189579699543,1.00000822963844),(1.,0.817605054849148,1.00000830175855),
(1.,0.812291861790874,1.00000854359006),(1.,0.808626740000292,1.00000871040914),
(1.,0.804766788192626,1.00000888609596)))
REPRESENTATION_ITEM('')
SURFACE()
);
#66=(
BOUNDED_SURFACE()
B_SPLINE_SURFACE(3,2,((#13786,#13787,#13788),(#13789,#13790,#13791),(#13792,
#13793,#13794),(#13795,#13796,#13797),(#13798,#13799,#13800),(#13801,#13802,
#13803),(#13804,#13805,#13806),(#13807,#13808,#13809)),.UNSPECIFIED.,.F.,
 .F.,.F.)
B_SPLINE_SURFACE_WITH_KNOTS((4,2,2,4),(3,3),(0.0461385444250929,0.0516992567704878,
0.0544796129431853,0.0572599691158827),(0.,1.00002275764377),
 .UNSPECIFIED.)
GEOMETRIC_REPRESENTATION_ITEM()
RATIONAL_B_SPLINE_SURFACE(((1.,0.804773725708297,1.00000888578001),(1.,
0.812372242905804,1.00000853993131),(1.,0.819062000811241,1.00000823544506),
(1.,0.819189579699735,1.00000822963827),(1.,0.817605054849233,1.00000830175837),
(1.,0.812291861790962,1.00000854358988),(1.,0.808626740000384,1.00000871040896),
(1.,0.804766788192718,1.00000888609577)))
REPRESENTATION_ITEM('')
SURFACE()
);
#67=(
BOUNDED_SURFACE()
B_SPLINE_SURFACE(3,2,((#13841,#13842,#13843),(#13844,#13845,#13846),(#13847,
#13848,#13849),(#13850,#13851,#13852),(#13853,#13854,#13855),(#13856,#13857,
#13858),(#13859,#13860,#13861),(#13862,#13863,#13864)),.UNSPECIFIED.,.F.,
 .F.,.F.)
B_SPLINE_SURFACE_WITH_KNOTS((4,2,2,4),(3,3),(0.0460112723212199,0.0515724236699156,
0.0543529993442635,0.0571335750186114),(0.,1.),.UNSPECIFIED.)
GEOMETRIC_REPRESENTATION_ITEM()
RATIONAL_B_SPLINE_SURFACE(((1.,0.804778149799748,1.),(1.,0.812377089679977,
1.),(1.,0.819066896577867,1.),(1.,0.81919332893791,1.),(1.,0.817608725913226,
1.),(1.,0.812295770981002,1.),(1.,0.808630931896093,1.),(1.,0.804771243949043,
1.)))
REPRESENTATION_ITEM('')
SURFACE()
);
#68=(
BOUNDED_SURFACE()
B_SPLINE_SURFACE(3,2,((#13896,#13897,#13898),(#13899,#13900,#13901),(#13902,
#13903,#13904),(#13905,#13906,#13907),(#13908,#13909,#13910),(#13911,#13912,
#13913),(#13914,#13915,#13916),(#13917,#13918,#13919)),.UNSPECIFIED.,.F.,
 .F.,.F.)
B_SPLINE_SURFACE_WITH_KNOTS((4,2,2,4),(3,3),(0.0459959130509696,0.0515565609914623,
0.0543368849617087,0.0571172089319551),(0.,1.00002218942476),
 .UNSPECIFIED.)
GEOMETRIC_REPRESENTATION_ITEM()
RATIONAL_B_SPLINE_SURFACE(((1.,0.804773845337407,1.00000866391214),(1.,
0.812372128424595,1.00000832670908),(1.,0.819061503960629,1.00000802984229),
(1.,0.81918996388213,1.00000802414138),(1.,0.81760551996088,1.00000809445718),
(1.,0.812292231605809,1.00000833025481),(1.,0.80862696186913,1.00000849291526),
(1.,0.804766890162773,1.0000086642208)))
REPRESENTATION_ITEM('')
SURFACE()
);
#69=(
BOUNDED_SURFACE()
B_SPLINE_SURFACE(3,2,((#13951,#13952,#13953),(#13954,#13955,#13956),(#13957,
#13958,#13959),(#13960,#13961,#13962),(#13963,#13964,#13965),(#13966,#13967,
#13968),(#13969,#13970,#13971),(#13972,#13973,#13974)),.UNSPECIFIED.,.F.,
 .F.,.F.)
B_SPLINE_SURFACE_WITH_KNOTS((4,2,2,4),(3,3),(0.0461385444250929,0.0516992567704878,
0.0544796129431853,0.0572599691158827),(0.,1.00002275764329),
 .UNSPECIFIED.)
GEOMETRIC_REPRESENTATION_ITEM()
RATIONAL_B_SPLINE_SURFACE(((1.,0.804773725708389,1.00000888577982),(1.,
0.812372242905893,1.00000853993114),(1.,0.819062000811328,1.00000823544489),
(1.,0.819189579699822,1.0000082296381),(1.,0.817605054849161,1.0000083017582),
(1.,0.812291861791211,1.00000854358971),(1.,0.808626740000355,1.00000871040877),
(1.,0.804766788192811,1.00000888609559)))
REPRESENTATION_ITEM('')
SURFACE()
);
#70=(
BOUNDED_SURFACE()
B_SPLINE_SURFACE(3,2,((#14006,#14007,#14008),(#14009,#14010,#14011),(#14012,
#14013,#14014),(#14015,#14016,#14017),(#14018,#14019,#14020),(#14021,#14022,
#14023),(#14024,#14025,#14026),(#14027,#14028,#14029)),.UNSPECIFIED.,.F.,
 .F.,.F.)
B_SPLINE_SURFACE_WITH_KNOTS((4,2,2,4),(3,3),(0.0461385444250929,0.0516992567704878,
0.0544796129431853,0.0572599691158827),(0.,1.00002275764337),
 .UNSPECIFIED.)
GEOMETRIC_REPRESENTATION_ITEM()
RATIONAL_B_SPLINE_SURFACE(((1.,0.804773725708374,1.00000888577985),(1.,
0.812372242905718,1.00000853993116),(1.,0.819062000811528,1.00000823544491),
(1.,0.8191895796997,1.00000822963813),(1.,0.817605054849307,1.00000830175823),
(1.,0.812291861791037,1.00000854358973),(1.,0.80862674000046,1.0000087104088),
(1.,0.804766788192796,1.00000888609562)))
REPRESENTATION_ITEM('')
SURFACE()
);
#71=TOROIDAL_SURFACE('',#3707,32.5,6.);
#72=TOROIDAL_SURFACE('',#3816,12.0720179162868,0.927982083713184);
#73=B_SPLINE_CURVE_WITH_KNOTS('',3,(#5793,#5794,#5795,#5796,#5797,#5798,
#5799,#5800,#5801,#5802,#5803,#5804),.UNSPECIFIED.,.F.,.F.,(4,2,2,2,2,4),
(-0.945051167958466,-0.841574089668648,-0.613708642186743,-0.375417318601337,
-0.18453510953063,0.),.UNSPECIFIED.);
#74=B_SPLINE_CURVE_WITH_KNOTS('',3,(#5810,#5811,#5812,#5813,#5814,#5815,
#5816,#5817,#5818,#5819,#5820,#5821,#5822,#5823,#5824,#5825,#5826,#5827,
#5828,#5829,#5830,#5831,#5832,#5833,#5834,#5835,#5836,#5837,#5838,#5839,
#5840,#5841,#5842,#5843,#5844,#5845),.UNSPECIFIED.,.F.,.F.,(4,2,2,2,2,2,
2,2,2,2,2,2,2,2,2,2,2,4),(-4.72701070515396,-4.58342020211309,-4.35573092128894,
-4.11738182551202,-3.88511531766138,-3.65439161452862,-3.41571207551833,
-3.18605838418004,-2.94775202391993,-2.71206608145108,-2.48446949005175,
-2.24614932091124,-2.01315165334969,-1.78371039541636,-1.54421591254515,
-1.3138550329973,-1.07808333104171,-0.945051167958466),.UNSPECIFIED.);
#75=B_SPLINE_CURVE_WITH_KNOTS('',3,(#5849,#5850,#5851,#5852,#5853,#5854,
#5855,#5856,#5857,#5858,#5859,#5860),.UNSPECIFIED.,.F.,.F.,(4,2,2,2,2,4),
(-100.860857186755,-100.719016322246,-100.572167893934,-100.332434988478,
-100.10326726078,-99.9157943215848),.UNSPECIFIED.);
#76=B_SPLINE_CURVE_WITH_KNOTS('',3,(#5865,#5866,#5867,#5868,#5869,#5870,
#5871,#5872,#5873,#5874,#5875,#5876,#5877,#5878,#5879,#5880,#5881,#5882,
#5883,#5884,#5885,#5886,#5887,#5888,#5889,#5890,#5891,#5892,#5893,#5894,
#5895,#5896,#5897,#5898,#5899,#5900),.UNSPECIFIED.,.F.,.F.,(4,2,2,2,2,2,
2,2,2,2,2,2,2,2,2,2,2,4),(-8.50901118085528,-8.32791893771986,-8.0990928267591,
-7.85910788244872,-7.62832437277772,-7.39390458531972,-7.15690768647293,
-6.92871712936123,-6.69044824129429,-6.45624357767479,-6.22815323543594,
-5.98733458562093,-5.75583554263634,-5.52335400543344,-5.28554117046482,
-5.05664510291043,-4.81833115193754,-4.72701070515396),.UNSPECIFIED.);
#77=B_SPLINE_CURVE_WITH_KNOTS('',3,(#5901,#5902,#5903,#5904,#5905,#5906,
#5907,#5908,#5909,#5910,#5911,#5912,#5913,#5914,#5915,#5916,#5917,#5918,
#5919,#5920,#5921,#5922,#5923,#5924,#5925,#5926,#5927,#5928,#5929,#5930,
#5931,#5932,#5933,#5934,#5935,#5936),.UNSPECIFIED.,.F.,.F.,(4,2,2,2,2,2,
2,2,2,2,2,2,2,2,2,2,2,4),(-99.9157943215848,-99.8700528920271,-99.6317245970861,
-99.4040778368149,-99.1681604611512,-98.9305377965158,-98.7006844014331,
-98.4617770049481,-98.2314058094206,-97.9989345477104,-97.7605772193135,
-97.5329301202136,-97.2978042552567,-97.0574907391568,-96.8283107464464,
-96.590175509048,-96.3583458899543,-96.1336669438351),.UNSPECIFIED.);
#78=B_SPLINE_CURVE_WITH_KNOTS('',3,(#5941,#5942,#5943,#5944,#5945,#5946,
#5947,#5948,#5949,#5950,#5951,#5952,#5953,#5954,#5955,#5956,#5957,#5958,
#5959,#5960,#5961,#5962,#5963,#5964,#5965,#5966,#5967,#5968,#5969,#5970,
#5971,#5972,#5973,#5974,#5975,#5976),.UNSPECIFIED.,.F.,.F.,(4,2,2,2,2,2,
2,2,2,2,2,2,2,2,2,2,2,4),(-12.2907867440871,-12.0718236771256,-11.8405116446575,
-11.602154571369,-11.3727826264931,-11.13338422805,-10.8980284551473,-10.670441358598,
-10.4321155432753,-10.1994280209644,-9.96950449632101,-9.73035393254469,
-9.50029148770774,-9.26352608944506,-9.02736214272124,-8.79965739283195,
-8.56136063203866,-8.50901118085528),.UNSPECIFIED.);
#79=B_SPLINE_CURVE_WITH_KNOTS('',3,(#5977,#5978,#5979,#5980,#5981,#5982,
#5983,#5984,#5985,#5986,#5987,#5988,#5989,#5990,#5991,#5992,#5993,#5994,
#5995,#5996,#5997,#5998,#5999,#6000,#6001,#6002,#6003,#6004,#6005,#6006,
#6007,#6008,#6009,#6010,#6011,#6012,#6013,#6014),.UNSPECIFIED.,.F.,.F.,
(4,2,2,2,2,2,2,2,2,2,2,2,2,2,2,2,2,2,4),(-96.1336669438351,-96.1265611334031,
-95.8881753300681,-95.6602076690697,-95.4257999831089,-95.1875195318992,
-94.9591189897511,-94.7218709411051,-94.4879625687659,-94.2569562534328,
-94.0167165913897,-93.7880836305017,-93.5544076599296,-93.3160825836461,
-93.0882520436014,-92.8518366239696,-92.6156796890001,-92.3853966159876,
-92.3513747143654),.UNSPECIFIED.);
#80=B_SPLINE_CURVE_WITH_KNOTS('',3,(#6019,#6020,#6021,#6022,#6023,#6024,
#6025,#6026,#6027,#6028,#6029,#6030,#6031,#6032,#6033,#6034,#6035,#6036,
#6037,#6038,#6039,#6040,#6041,#6042,#6043,#6044,#6045,#6046,#6047,#6048,
#6049,#6050,#6051,#6052,#6053,#6054,#6055,#6056),.UNSPECIFIED.,.F.,.F.,
(4,2,2,2,2,2,2,2,2,2,2,2,2,2,2,2,2,2,4),(-16.0726421798861,-16.0448513456216,
-15.8143696875198,-15.5789960071959,-15.3423470933369,-15.1144009066226,
-14.8761154158147,-14.6422274147382,-14.4138663966335,-14.1733928484136,
-13.9421888767155,-13.708935835368,-13.4714587727836,-13.2428582790979,
-13.0045799578113,-12.7699694473923,-12.5421573893674,-12.3038028906354,
-12.2907867440871),.UNSPECIFIED.);
#81=B_SPLINE_CURVE_WITH_KNOTS('',3,(#6057,#6058,#6059,#6060,#6061,#6062,
#6063,#6064,#6065,#6066,#6067,#6068,#6069,#6070,#6071,#6072,#6073,#6074,
#6075,#6076,#6077,#6078,#6079,#6080,#6081,#6082,#6083,#6084,#6085,#6086,
#6087,#6088,#6089,#6090,#6091,#6092),.UNSPECIFIED.,.F.,.F.,(4,2,2,2,2,2,
2,2,2,2,2,2,2,2,2,2,2,4),(-92.3513747143654,-92.1459953794631,-91.9163548635556,
-91.6834391927834,-91.4450851548889,-91.2174685300907,-90.9818718133715,
-90.7431410078649,-90.5135598140373,-90.2749665782474,-90.044002763264,
-89.8118106876991,-89.5734277997817,-89.345669086319,-89.110837285638,-88.8725049462534,
-88.6436870106884,-88.5689774530533),.UNSPECIFIED.);
#82=B_SPLINE_CURVE_WITH_KNOTS('',3,(#6097,#6098,#6099,#6100,#6101,#6102,
#6103,#6104,#6105,#6106,#6107,#6108,#6109,#6110,#6111,#6112,#6113,#6114,
#6115,#6116,#6117,#6118,#6119,#6120,#6121,#6122,#6123,#6124,#6125,#6126,
#6127,#6128,#6129,#6130,#6131,#6132),.UNSPECIFIED.,.F.,.F.,(4,2,2,2,2,2,
2,2,2,2,2,2,2,2,2,2,2,4),(-19.8545421250936,-19.7886210374653,-19.5595194352788,
-19.3189557440687,-19.0839201041549,-18.8562708334143,-18.6179276836627,
-18.3855426708408,-18.1550554085007,-17.9162429867753,-17.6864737489498,
-17.4486140745901,-17.2127927161367,-16.9851780130659,-16.746863863508,
-16.5137398595355,-16.2844857040836,-16.0726421798861),.UNSPECIFIED.);
#83=B_SPLINE_CURVE_WITH_KNOTS('',3,(#6133,#6134,#6135,#6136,#6137,#6138,
#6139,#6140,#6141,#6142,#6143,#6144,#6145,#6146,#6147,#6148,#6149,#6150,
#6151,#6152,#6153,#6154,#6155,#6156,#6157,#6158,#6159,#6160,#6161,#6162,
#6163,#6164,#6165,#6166,#6167,#6168),.UNSPECIFIED.,.F.,.F.,(4,2,2,2,2,2,
2,2,2,2,2,2,2,2,2,2,2,4),(-88.5689774530533,-88.4059660126083,-88.1731764713921,
-87.9417553066357,-87.7010318555137,-87.4728183271102,-87.2386994385408,
-87.000392596865,-86.7722693783642,-86.5353697816887,-86.3005728167057,
-86.0698705375273,-85.8299838138407,-85.6009757129622,-85.3676210877026,
-85.129286020926,-84.9015921002416,-84.7864811960255),.UNSPECIFIED.);
#84=B_SPLINE_CURVE_WITH_KNOTS('',3,(#6173,#6174,#6175,#6176,#6177,#6178,
#6179,#6180,#6181,#6182,#6183,#6184,#6185,#6186,#6187,#6188,#6189,#6190,
#6191,#6192,#6193,#6194,#6195,#6196,#6197,#6198,#6199,#6200,#6201,#6202,
#6203,#6204,#6205,#6206,#6207,#6208),.UNSPECIFIED.,.F.,.F.,(4,2,2,2,2,2,
2,2,2,2,2,2,2,2,2,2,2,4),(-23.6364428905114,-23.5280727188282,-23.3003170968824,
-23.0620315711668,-22.8284660746515,-22.599797428317,-22.3596760760626,
-22.1287758117826,-21.8947223471241,-21.6575908713894,-21.4292896926289,
-21.1910315806139,-20.9567054769666,-20.7287091966259,-20.4903376329144,
-20.2586320072491,-20.0266683991165,-19.8545421250936),.UNSPECIFIED.);
#85=B_SPLINE_CURVE_WITH_KNOTS('',3,(#6209,#6210,#6211,#6212,#6213,#6214,
#6215,#6216,#6217,#6218,#6219,#6220,#6221,#6222,#6223,#6224,#6225,#6226,
#6227,#6228,#6229,#6230,#6231,#6232,#6233,#6234,#6235,#6236,#6237,#6238,
#6239,#6240,#6241,#6242,#6243,#6244),.UNSPECIFIED.,.F.,.F.,(4,2,2,2,2,2,
2,2,2,2,2,2,2,2,2,2,2,4),(-84.7864811960255,-84.6655244516862,-84.4283266068344,
-84.1983430392082,-83.9592870567852,-83.7291292347511,-83.4965240136712,
-83.2581598823036,-83.0305262715843,-82.795259343992,-82.5553979452392,
-82.3260971111831,-82.0878248655658,-81.8562429676943,-81.6243359927227,
-81.3859432768132,-81.1580373792479,-81.0040618503967),.UNSPECIFIED.);
#86=B_SPLINE_CURVE_WITH_KNOTS('',3,(#6249,#6250,#6251,#6252,#6253,#6254,
#6255,#6256,#6257,#6258,#6259,#6260,#6261,#6262,#6263,#6264,#6265,#6266,
#6267,#6268,#6269,#6270,#6271,#6272,#6273,#6274,#6275,#6276,#6277,#6278,
#6279,#6280,#6281,#6282,#6283,#6284),.UNSPECIFIED.,.F.,.F.,(4,2,2,2,2,2,
2,2,2,2,2,2,2,2,2,2,2,4),(-27.4182083858629,-27.2701824506046,-27.0424357273862,
-26.8040924069698,-26.5720037208871,-26.340949280599,-26.1024683172712,
-25.8729888257624,-25.634057144684,-25.3985738820072,-25.1709986113392,
-24.9326840817343,-24.6998769564909,-24.4701692126494,-24.2308851039948,
-24.0007075184348,-23.7643712325812,-23.6364428905114),.UNSPECIFIED.);
#87=B_SPLINE_CURVE_WITH_KNOTS('',3,(#6285,#6286,#6287,#6288,#6289,#6290,
#6291,#6292,#6293,#6294,#6295,#6296,#6297,#6298,#6299,#6300,#6301,#6302,
#6303,#6304,#6305,#6306,#6307,#6308,#6309,#6310,#6311,#6312,#6313,#6314,
#6315,#6316,#6317,#6318,#6319,#6320),.UNSPECIFIED.,.F.,.F.,(4,2,2,2,2,2,
2,2,2,2,2,2,2,2,2,2,2,4),(-81.0040618503967,-80.92350308096,-80.6852010443942,
-80.4566759266639,-80.2192876137424,-79.9856970630905,-79.7545672730092,
-79.5141847658083,-79.2856734462051,-79.0518665659799,-78.8135388051234,
-78.5856317966836,-78.3490744232575,-78.113299330973,-77.8828928362824,
-77.643349760312,-77.413888713748,-77.2215001553636),.UNSPECIFIED.);
#88=B_SPLINE_CURVE_WITH_KNOTS('',3,(#6325,#6326,#6327,#6328,#6329,#6330,
#6331,#6332,#6333,#6334,#6335,#6336,#6337,#6338,#6339,#6340,#6341,#6342,
#6343,#6344,#6345,#6346,#6347,#6348,#6349,#6350,#6351,#6352,#6353,#6354,
#6355,#6356,#6357,#6358,#6359,#6360),.UNSPECIFIED.,.F.,.F.,(4,2,2,2,2,2,
2,2,2,2,2,2,2,2,2,2,2,4),(-31.2000580417808,-31.0140725636771,-30.7850089289431,
-30.5452410020026,-30.3146451340147,-30.079677015553,-29.8428951155429,
-29.6148653852519,-29.3765956140283,-29.1425869882947,-28.9143527457507,
-28.6737469858917,-28.4424308234987,-28.2095103262391,-27.9719044243992,
-27.7431911460644,-27.5049074861638,-27.4182083858629),.UNSPECIFIED.);
#89=B_SPLINE_CURVE_WITH_KNOTS('',3,(#6361,#6362,#6363,#6364,#6365,#6366,
#6367,#6368,#6369,#6370,#6371,#6372,#6373,#6374,#6375,#6376,#6377,#6378,
#6379,#6380,#6381,#6382,#6383,#6384,#6385,#6386,#6387,#6388,#6389,#6390,
#6391,#6392,#6393,#6394,#6395,#6396,#6397,#6398),.UNSPECIFIED.,.F.,.F.,
(4,2,2,2,2,2,2,2,2,2,2,2,2,2,2,2,2,2,4),(-77.2215001553636,-77.1808445817772,
-76.9424879838381,-76.7148550360144,-76.4791214839487,-76.24081517708,-76.0111164482566,
-75.7723890603129,-75.5416493168672,-75.309337139177,-75.0709516032645,
-74.8432306674689,-74.6082731469132,-74.3699212863644,-74.1409797468126,
-73.9031186514559,-73.6706272268202,-73.4390822861619,-73.4390542992583),
 .UNSPECIFIED.);
#90=B_SPLINE_CURVE_WITH_KNOTS('',3,(#6403,#6404,#6405,#6406,#6407,#6408,
#6409,#6410,#6411,#6412,#6413,#6414,#6415,#6416,#6417,#6418,#6419,#6420,
#6421,#6422,#6423,#6424,#6425,#6426,#6427,#6428,#6429,#6430,#6431,#6432,
#6433,#6434,#6435,#6436,#6437,#6438),.UNSPECIFIED.,.F.,.F.,(4,2,2,2,2,2,
2,2,2,2,2,2,2,2,2,2,2,4),(-34.9817405379481,-34.7583828467543,-34.5266960718299,
-34.2885333255229,-34.0593317151714,-33.8192528633057,-33.5840972266921,
-33.3564889441506,-33.1181617298444,-32.8856634252833,-32.6554200731001,
-32.4164800124183,-32.1866008400906,-31.949200980976,-31.7132497196655,
-31.4856149669365,-31.2473168000567,-31.2000580417808),.UNSPECIFIED.);
#91=B_SPLINE_CURVE_WITH_KNOTS('',3,(#6439,#6440,#6441,#6442,#6443,#6444,
#6445,#6446,#6447,#6448,#6449,#6450,#6451,#6452,#6453,#6454,#6455,#6456,
#6457,#6458,#6459,#6460,#6461,#6462,#6463,#6464,#6465,#6466,#6467,#6468,
#6469,#6470,#6471,#6472,#6473,#6474),.UNSPECIFIED.,.F.,.F.,(4,2,2,2,2,2,
2,2,2,2,2,2,2,2,2,2,2,4),(-73.4390542992583,-73.1982145373766,-72.9700975195046,
-72.7358457406193,-72.4975408236058,-72.2693054491002,-72.0322598549638,
-71.7978365151172,-71.5670068623664,-71.3269726164317,-71.0981253205832,
-70.8646364649506,-70.6263037079221,-70.3985595539543,-70.1623470914066,
-69.9255831849977,-69.6954748942385,-69.6566458982394),.UNSPECIFIED.);
#92=B_SPLINE_CURVE_WITH_KNOTS('',3,(#6479,#6480,#6481,#6482,#6483,#6484,
#6485,#6486,#6487,#6488,#6489,#6490,#6491,#6492,#6493,#6494,#6495,#6496,
#6497,#6498,#6499,#6500,#6501,#6502,#6503,#6504,#6505,#6506,#6507,#6508,
#6509,#6510,#6511,#6512,#6513,#6514,#6515,#6516),.UNSPECIFIED.,.F.,.F.,
(4,2,2,2,2,2,2,2,2,2,2,2,2,2,2,2,2,2,4),(-38.7635679894171,-38.730951426609,
-38.5006459899062,-38.2646912803571,-38.0282461533568,-37.8004147265788,
-37.5621215735029,-37.3284203348966,-37.0998739613677,-36.8596046467075,
-36.6285759264362,-36.3948415542348,-36.1575645239461,-35.9291406831464,
-35.6908838834915,-35.4564528376755,-35.2285451591809,-34.9901894258272,
-34.9817405379481),.UNSPECIFIED.);
#93=B_SPLINE_CURVE_WITH_KNOTS('',3,(#6517,#6518,#6519,#6520,#6521,#6522,
#6523,#6524,#6525,#6526,#6527,#6528,#6529,#6530,#6531,#6532,#6533,#6534,
#6535,#6536,#6537,#6538,#6539,#6540,#6541,#6542,#6543,#6544,#6545,#6546,
#6547,#6548,#6549,#6550,#6551,#6552),.UNSPECIFIED.,.F.,.F.,(4,2,2,2,2,2,
2,2,2,2,2,2,2,2,2,2,2,4),(-69.6566458982394,-69.4562754604573,-69.2263356551233,
-68.9936015034485,-68.7552396899331,-68.5276187183144,-68.292215225518,
-68.052821027123,-67.8234040515846,-67.5849991258093,-67.353674141074,-67.1216493381286,
-66.8832588270564,-66.6554174863463,-66.4207605499414,-66.1824448046608,
-65.9537989682913,-65.8742130838229),.UNSPECIFIED.);
#94=B_SPLINE_CURVE_WITH_KNOTS('',3,(#6557,#6558,#6559,#6560,#6561,#6562,
#6563,#6564,#6565,#6566,#6567,#6568,#6569,#6570,#6571,#6572,#6573,#6574,
#6575,#6576,#6577,#6578,#6579,#6580,#6581,#6582,#6583,#6584,#6585,#6586,
#6587,#6588,#6589,#6590,#6591,#6592),.UNSPECIFIED.,.F.,.F.,(4,2,2,2,2,2,
2,2,2,2,2,2,2,2,2,2,2,4),(-42.5454845738913,-42.4722250372372,-42.2433846535402,
-42.0050768911068,-41.7702225547603,-41.5425130766005,-41.304162127578,
-41.0719495737161,-40.8411173069286,-40.6024982836502,-40.3728973337731,
-40.1343873884848,-39.8987632388426,-39.6711722063643,-39.4328501439237,
-39.1999103036718,-38.9703818511288,-38.7635679894171),.UNSPECIFIED.);
#95=B_SPLINE_CURVE_WITH_KNOTS('',3,(#6593,#6594,#6595,#6596,#6597,#6598,
#6599,#6600,#6601,#6602,#6603,#6604,#6605,#6606,#6607,#6608,#6609,#6610,
#6611,#6612,#6613,#6614,#6615,#6616,#6617,#6618,#6619,#6620,#6621,#6622,
#6623,#6624,#6625,#6626,#6627,#6628),.UNSPECIFIED.,.F.,.F.,(4,2,2,2,2,2,
2,2,2,2,2,2,2,2,2,2,2,4),(-65.8742130838229,-65.7162737876648,-65.4830140253136,
-65.2517643749619,-65.0112419678356,-64.7828569895144,-64.5489221737502,
-64.3106010757685,-64.0826126583152,-63.8459154416866,-63.6105409825893,
-63.3800136247092,-63.1403304694885,-62.9110577329829,-62.6778871130127,
-62.4395373717821,-62.2118860415347,-62.0916342174998),.UNSPECIFIED.);
#96=B_SPLINE_CURVE_WITH_KNOTS('',3,(#6633,#6634,#6635,#6636,#6637,#6638,
#6639,#6640,#6641,#6642,#6643,#6644,#6645,#6646,#6647,#6648,#6649,#6650,
#6651,#6652,#6653,#6654,#6655,#6656,#6657,#6658,#6659,#6660,#6661,#6662,
#6663,#6664,#6665,#6666,#6667,#6668),.UNSPECIFIED.,.F.,.F.,(4,2,2,2,2,2,
2,2,2,2,2,2,2,2,2,2,2,4),(-46.3274862212502,-46.2139349710691,-45.9862520631046,
-45.7479510822666,-45.514570222929,-45.2856655043703,-45.0457476103363,
-44.8150216716406,-44.5804220517271,-44.3434914755233,-44.1153521114665,
-43.877079193963,-43.642934622709,-43.4147962866385,-43.1740430399489,-42.9425997608968,
-42.7099744625215,-42.5454845738913),.UNSPECIFIED.);
#97=B_SPLINE_CURVE_WITH_KNOTS('',3,(#6669,#6670,#6671,#6672,#6673,#6674,
#6675,#6676,#6677,#6678,#6679,#6680,#6681,#6682,#6683,#6684,#6685,#6686,
#6687,#6688,#6689,#6690,#6691,#6692,#6693,#6694,#6695,#6696,#6697,#6698,
#6699,#6700,#6701,#6702,#6703,#6704),.UNSPECIFIED.,.F.,.F.,(4,2,2,2,2,2,
2,2,2,2,2,2,2,2,2,2,2,4),(-62.0916342174998,-61.9760168268649,-61.7381605371751,
-61.5083461244539,-61.2694855976273,-61.0389840970219,-60.80655322902,-60.5681744778011,
-60.3404938262001,-60.1054113560928,-59.8648525874502,-59.6357068116143,
-59.3976125670906,-59.1656371959061,-58.9338869248346,-58.6954797464671,
-58.4674560570048,-58.3090769307648),.UNSPECIFIED.);
#98=B_SPLINE_CURVE_WITH_KNOTS('',3,(#6709,#6710,#6711,#6712,#6713,#6714,
#6715,#6716,#6717,#6718,#6719,#6720,#6721,#6722,#6723,#6724,#6725,#6726,
#6727,#6728,#6729,#6730,#6731,#6732,#6733,#6734,#6735,#6736,#6737,#6738,
#6739,#6740,#6741,#6742,#6743,#6744),.UNSPECIFIED.,.F.,.F.,(4,2,2,2,2,2,
2,2,2,2,2,2,2,2,2,2,2,4),(-50.1093942211471,-49.9567830768948,-49.7289379381517,
-49.4905792650358,-49.2586532650307,-49.0272163525885,-48.7889194778806,
-48.5595999453668,-48.3199763649759,-48.0846826473659,-47.857087398902,
-47.6187573557871,-47.3861282487955,-47.156098687667,-46.9170133518871,
-46.6870073167293,-46.4500330423276,-46.3274862212502),.UNSPECIFIED.);
#99=B_SPLINE_CURVE_WITH_KNOTS('',3,(#6745,#6746,#6747,#6748,#6749,#6750,
#6751,#6752,#6753,#6754,#6755,#6756,#6757,#6758,#6759,#6760,#6761,#6762,
#6763,#6764,#6765,#6766,#6767,#6768,#6769,#6770,#6771,#6772,#6773,#6774,
#6775,#6776,#6777,#6778,#6779,#6780),.UNSPECIFIED.,.F.,.F.,(4,2,2,2,2,2,
2,2,2,2,2,2,2,2,2,2,2,4),(-58.3090769307648,-58.2330845708498,-57.994791177349,
-57.7664459669195,-57.5292676010225,-57.295207858664,-57.064263082704,-56.8240942169975,
-56.595403200837,-56.3617921973811,-56.1234714272172,-55.8956766402114,
-55.6593313097667,-55.4229936465461,-55.1927717434584,-54.9534404271447,
-54.7237149766201,-54.5267363962688),.UNSPECIFIED.);
#100=B_SPLINE_CURVE_WITH_KNOTS('',3,(#6785,#6786,#6787,#6788,#6789,#6790,
#6791,#6792,#6793,#6794,#6795,#6796,#6797,#6798,#6799,#6800,#6801,#6802,
#6803,#6804,#6805,#6806,#6807,#6808,#6809,#6810,#6811,#6812,#6813,#6814,
#6815,#6816,#6817,#6818,#6819,#6820),.UNSPECIFIED.,.F.,.F.,(4,2,2,2,2,2,
2,2,2,2,2,2,2,2,2,2,2,4),(-53.8914326771441,-53.6942463180612,-53.4641320716806,
-53.231536971558,-52.9931960827502,-52.765586112647,-52.5290010051772,-52.30109163005,
-52.0627998313959,-51.828969941831,-51.6005463821193,-51.3601365561174,
-51.1289868370583,-50.8955735447212,-50.6581587562352,-50.4296129262629,
-50.1913380824163,-50.1093942211471),.UNSPECIFIED.);
#101=B_SPLINE_CURVE_WITH_KNOTS('',3,(#6821,#6822,#6823,#6824,#6825,#6826,
#6827,#6828,#6829,#6830,#6831,#6832,#6833,#6834,#6835,#6836,#6837,#6838,
#6839,#6840,#6841,#6842,#6843,#6844,#6845,#6846,#6847,#6848,#6849,#6850,
#6851,#6852,#6853,#6854,#6855,#6856),.UNSPECIFIED.,.F.,.F.,(4,2,2,2,2,2,
2,2,2,2,2,2,2,2,2,2,2,4),(-54.5267363962688,-54.4908627524364,-54.2525129803029,
-54.0249036906896,-53.7893742600372,-53.5504440838935,-53.3209209565464,
-53.0823936458037,-52.8534147673518,-52.6135121188718,-52.382796618409,
-52.1480599607188,-51.911144561536,-51.6830108878803,-51.4447097678497,
-51.2105768919698,-50.9823832511243,-50.744421786252),.UNSPECIFIED.);
#102=B_SPLINE_CURVE_WITH_KNOTS('',3,(#6861,#6862,#6863,#6864,#6865,#6866,
#6867,#6868,#6869,#6870,#6871,#6872,#6873,#6874,#6875,#6876,#6877,#6878,
#6879,#6880,#6881,#6882,#6883,#6884,#6885,#6886,#6887,#6888,#6889,#6890,
#6891,#6892,#6893,#6894,#6895,#6896),.UNSPECIFIED.,.F.,.F.,(4,2,2,2,2,2,
2,2,2,2,2,2,2,2,2,2,2,4),(-57.6734244832962,-57.4356455965062,-57.207463872803,
-56.9733547726644,-56.7350711356582,-56.5069595853773,-56.2700688004548,
-56.0353309893982,-55.8046387301499,-55.5647609815634,-55.3357909413717,
-55.1024459514368,-54.864134125454,-54.6364578442597,-54.400399095822,-54.163266274685,
-53.9332929597696,-53.8914326771441),.UNSPECIFIED.);
#103=B_SPLINE_CURVE_WITH_KNOTS('',3,(#6897,#6898,#6899,#6900,#6901,#6902,
#6903,#6904,#6905,#6906,#6907,#6908,#6909,#6910,#6911,#6912,#6913,#6914,
#6915,#6916,#6917,#6918,#6919,#6920,#6921,#6922,#6923,#6924,#6925,#6926,
#6927,#6928,#6929,#6930,#6931,#6932,#6933,#6934),.UNSPECIFIED.,.F.,.F.,
(4,2,2,2,2,2,2,2,2,2,2,2,2,2,2,2,2,2,4),(-50.744421786252,-50.7416442860852,
-50.5102103743226,-50.2774702301927,-50.0397342334648,-49.8109034923061,
-49.5725737752064,-49.3377290004435,-49.1099815298265,-48.8716037031331,
-48.63939939237,-48.4084741501181,-48.1698667577858,-47.9402736227072,-47.7016109703721,
-47.4659996105955,-47.2383863882127,-47.0000374246888,-46.9621556460553),
 .UNSPECIFIED.);
#104=B_SPLINE_CURVE_WITH_KNOTS('',3,(#6939,#6940,#6941,#6942,#6943,#6944,
#6945,#6946,#6947,#6948,#6949,#6950,#6951,#6952,#6953,#6954,#6955,#6956,
#6957,#6958,#6959,#6960,#6961,#6962,#6963,#6964,#6965,#6966,#6967,#6968,
#6969,#6970,#6971,#6972,#6973,#6974,#6975,#6976),.UNSPECIFIED.,.F.,.F.,
(4,2,2,2,2,2,2,2,2,2,2,2,2,2,2,2,2,2,4),(-61.4554063830696,-61.4176876659541,
-61.1793564073111,-60.9517606003038,-60.7161733529179,-60.4775072406849,
-60.2479368198683,-60.0093536212889,-59.7784342335843,-59.5462529494306,
-59.3078928343578,-59.0801601502359,-58.8453388664692,-58.6070276784985,
-58.3782198817519,-58.140508292822,-57.9077705088657,-57.6763597347384,
-57.6734244832962),.UNSPECIFIED.);
#105=B_SPLINE_CURVE_WITH_KNOTS('',3,(#6977,#6978,#6979,#6980,#6981,#6982,
#6983,#6984,#6985,#6986,#6987,#6988,#6989,#6990,#6991,#6992,#6993,#6994,
#6995,#6996,#6997,#6998,#6999,#7000,#7001,#7002,#7003,#7004,#7005,#7006,
#7007,#7008,#7009,#7010,#7011,#7012),.UNSPECIFIED.,.F.,.F.,(4,2,2,2,2,2,
2,2,2,2,2,2,2,2,2,2,2,4),(-46.9621556460553,-46.7671082522818,-46.5374999065735,
-46.2980833389991,-46.0677874195046,-45.8316925770558,-45.5952617136895,
-45.3674257432928,-45.129105725766,-44.8954158475436,-44.6668066136594,
-44.4265514218191,-44.1955322085225,-43.9616766247489,-43.7244133311704,
-43.4959996459181,-43.2577215083365,-43.1798021454525),.UNSPECIFIED.);
#106=B_SPLINE_CURVE_WITH_KNOTS('',3,(#7017,#7018,#7019,#7020,#7021,#7022,
#7023,#7024,#7025,#7026,#7027,#7028,#7029,#7030,#7031,#7032,#7033,#7034,
#7035,#7036,#7037,#7038,#7039,#7040,#7041,#7042,#7043,#7044,#7045,#7046,
#7047,#7048,#7049,#7050,#7051,#7052),.UNSPECIFIED.,.F.,.F.,(4,2,2,2,2,2,
2,2,2,2,2,2,2,2,2,2,2,4),(-65.2374739513206,-65.1597137841198,-64.9214542750747,
-64.6930636066121,-64.4558247570368,-64.2219705028162,-63.9909744370199,
-63.7507440295899,-63.5221454619045,-63.2884792888966,-63.0501769792657,
-62.8223614114859,-62.5859549937987,-62.3498585298257,-62.1195856839448,
-61.8801937683809,-61.6505933291242,-61.4554063830696),.UNSPECIFIED.);
#107=B_SPLINE_CURVE_WITH_KNOTS('',3,(#7053,#7054,#7055,#7056,#7057,#7058,
#7059,#7060,#7061,#7062,#7063,#7064,#7065,#7066,#7067,#7068,#7069,#7070,
#7071,#7072,#7073,#7074,#7075,#7076,#7077,#7078,#7079,#7080,#7081,#7082,
#7083,#7084,#7085,#7086,#7087,#7088),.UNSPECIFIED.,.F.,.F.,(4,2,2,2,2,2,
2,2,2,2,2,2,2,2,2,2,2,4),(-43.1798021454525,-43.0233005184053,-42.7953477083257,
-42.5569663446575,-42.3251688520465,-42.0933816876821,-41.8552316604598,
-41.6260390539229,-41.3857985088062,-41.1506571598224,-40.9230178905739,
-40.6846650171423,-40.4521792375946,-40.2218455910818,-39.9829216392961,
-39.7530542026248,-39.5155007168095,-39.3976161936097),.UNSPECIFIED.);
#108=B_SPLINE_CURVE_WITH_KNOTS('',3,(#7093,#7094,#7095,#7096,#7097,#7098,
#7099,#7100,#7101,#7102,#7103,#7104,#7105,#7106,#7107,#7108,#7109,#7110,
#7111,#7112,#7113,#7114,#7115,#7116,#7117,#7118,#7119,#7120,#7121,#7122,
#7123,#7124,#7125,#7126,#7127,#7128),.UNSPECIFIED.,.F.,.F.,(4,2,2,2,2,2,
2,2,2,2,2,2,2,2,2,2,2,4),(-69.019372509275,-68.9016766044539,-68.6641192632124,
-68.434275259458,-68.1953763224697,-67.9650488487731,-67.7325868762516,
-67.4942519163572,-67.266628578738,-67.0315115784664,-66.7912661109365,
-66.5620964052668,-66.3239707395895,-66.0921882104742,-65.8604138727514,
-65.6220504300927,-65.3941112139331,-65.2374739513206),.UNSPECIFIED.);
#109=B_SPLINE_CURVE_WITH_KNOTS('',3,(#7129,#7130,#7131,#7132,#7133,#7134,
#7135,#7136,#7137,#7138,#7139,#7140,#7141,#7142,#7143,#7144,#7145,#7146,
#7147,#7148,#7149,#7150,#7151,#7152,#7153,#7154,#7155,#7156,#7157,#7158,
#7159,#7160,#7161,#7162,#7163,#7164),.UNSPECIFIED.,.F.,.F.,(4,2,2,2,2,2,
2,2,2,2,2,2,2,2,2,2,2,4),(-39.3976161936097,-39.2795664375483,-39.0519185558299,
-38.8135947219172,-38.580364848747,-38.3512267997343,-38.1114765039187,
-37.8808934389617,-37.6457880904805,-37.4090238643793,-37.1809993170469,
-36.9427039654236,-36.7087096301277,-36.4804196120852,-36.2398308864171,
-36.0085267678092,-35.7754906149688,-35.6153851283096),.UNSPECIFIED.);
#110=B_SPLINE_CURVE_WITH_KNOTS('',3,(#7169,#7170,#7171,#7172,#7173,#7174,
#7175,#7176,#7177,#7178,#7179,#7180,#7181,#7182,#7183,#7184,#7185,#7186,
#7187,#7188,#7189,#7190,#7191,#7192,#7193,#7194,#7195,#7196,#7197,#7198,
#7199,#7200,#7201,#7202,#7203,#7204),.UNSPECIFIED.,.F.,.F.,(4,2,2,2,2,2,
2,2,2,2,2,2,2,2,2,2,2,4),(-72.8013143187673,-72.6413921294953,-72.4083580675375,
-72.1770775857943,-71.9365142073292,-71.7082359793028,-71.4742659088467,
-71.2359884777822,-71.0079860078507,-70.771246873831,-70.5361401782511,
-70.3055808023638,-70.0658558659785,-69.8367265402269,-69.6035208632225,
-69.3652149385238,-69.1375859965796,-69.019372509275),.UNSPECIFIED.);
#111=B_SPLINE_CURVE_WITH_KNOTS('',3,(#7205,#7206,#7207,#7208,#7209,#7210,
#7211,#7212,#7213,#7214,#7215,#7216,#7217,#7218,#7219,#7220,#7221,#7222,
#7223,#7224,#7225,#7226,#7227,#7228,#7229,#7230,#7231,#7232,#7233,#7234,
#7235,#7236,#7237,#7238,#7239,#7240),.UNSPECIFIED.,.F.,.F.,(4,2,2,2,2,2,
2,2,2,2,2,2,2,2,2,2,2,4),(-35.6153851283096,-35.5379009882013,-35.3092001135616,
-35.0708970177155,-34.8361843624883,-34.6083995726921,-34.3700319850573,
-34.137954416543,-33.9068062025092,-33.668339927752,-33.4388711908287,-33.1997849001402,
-32.96431758397,-32.736719856299,-32.4983810318796,-32.2655877758767,-32.0357987356091,
-31.8332798855205),.UNSPECIFIED.);
#112=B_SPLINE_CURVE_WITH_KNOTS('',3,(#7245,#7246,#7247,#7248,#7249,#7250,
#7251,#7252,#7253,#7254,#7255,#7256,#7257,#7258,#7259,#7260,#7261,#7262,
#7263,#7264,#7265,#7266,#7267,#7268,#7269,#7270,#7271,#7272,#7273,#7274,
#7275,#7276,#7277,#7278,#7279,#7280),.UNSPECIFIED.,.F.,.F.,(4,2,2,2,2,2,
2,2,2,2,2,2,2,2,2,2,2,4),(-76.5831287300173,-76.3807946254889,-76.1510131669601,
-75.918244010913,-75.6799233281813,-75.4523429669146,-75.2169003495295,
-74.9778100888382,-74.7483646077869,-74.5099230950359,-74.2787804977059,
-74.0467264872251,-73.8083770487214,-73.580607008871,-73.3459183688024,
-73.1076342303079,-72.8789568137339,-72.8013143187673),.UNSPECIFIED.);
#113=B_SPLINE_CURVE_WITH_KNOTS('',3,(#7281,#7282,#7283,#7284,#7285,#7286,
#7287,#7288,#7289,#7290,#7291,#7292,#7293,#7294,#7295,#7296,#7297,#7298,
#7299,#7300,#7301,#7302,#7303,#7304,#7305,#7306,#7307,#7308,#7309,#7310,
#7311,#7312,#7313,#7314,#7315,#7316,#7317,#7318),.UNSPECIFIED.,.F.,.F.,
(4,2,2,2,2,2,2,2,2,2,2,2,2,2,2,2,2,2,4),(-31.8332798855205,-31.7965319071712,
-31.5663670970833,-31.3298877331002,-31.093607007729,-30.8658469576634,
-30.6275371592618,-30.39398655729,-30.1652536288997,-29.9251501787876,-29.6942629804963,
-29.4600849911831,-29.222971107908,-28.9946824297206,-28.7564001881208,
-28.5220881224759,-28.294045785471,-28.0556511973426,-28.051200537517),
 .UNSPECIFIED.);
#114=B_SPLINE_CURVE_WITH_KNOTS('',3,(#7323,#7324,#7325,#7326,#7327,#7328,
#7329,#7330,#7331,#7332,#7333,#7334,#7335,#7336,#7337,#7338,#7339,#7340,
#7341,#7342,#7343,#7344,#7345,#7346,#7347,#7348,#7349,#7350,#7351,#7352,
#7353,#7354,#7355,#7356,#7357,#7358,#7359,#7360),.UNSPECIFIED.,.F.,.F.,
(4,2,2,2,2,2,2,2,2,2,2,2,2,2,2,2,2,2,4),(-80.3649154835294,-80.3606244670685,
-80.1222482405985,-79.8942192990533,-79.6599315218819,-79.4216674436202,
-79.1934021475701,-78.9563134160552,-78.7221360441692,-78.4912726435801,
-78.251194673345,-78.0224721048771,-77.7889458569104,-77.5506542008286,
-77.3229145925487,-77.086658964388,-76.8501773059356,-76.62003616798,-76.5831287300173),
 .UNSPECIFIED.);
#115=B_SPLINE_CURVE_WITH_KNOTS('',3,(#7361,#7362,#7363,#7364,#7365,#7366,
#7367,#7368,#7369,#7370,#7371,#7372,#7373,#7374,#7375,#7376,#7377,#7378,
#7379,#7380,#7381,#7382,#7383,#7384,#7385,#7386,#7387,#7388,#7389,#7390,
#7391,#7392,#7393,#7394,#7395,#7396),.UNSPECIFIED.,.F.,.F.,(4,2,2,2,2,2,
2,2,2,2,2,2,2,2,2,2,2,4),(-28.051200537517,-27.8239586602662,-27.5918911071802,
-27.3538607998307,-27.1247722659998,-26.8840400858967,-26.6490232225647,
-26.4213420375868,-26.1829758350914,-25.9506078282134,-25.7200260903725,
-25.4812346407419,-25.2514816603531,-25.0134603157911,-24.7776609496024,
-24.5500328914262,-24.3116956709026,-24.2689961176951),.UNSPECIFIED.);
#116=B_SPLINE_CURVE_WITH_KNOTS('',3,(#7401,#7402,#7403,#7404,#7405,#7406,
#7407,#7408,#7409,#7410,#7411,#7412,#7413,#7414,#7415,#7416,#7417,#7418,
#7419,#7420,#7421,#7422,#7423,#7424,#7425,#7426,#7427,#7428,#7429,#7430,
#7431,#7432,#7433,#7434,#7435,#7436),.UNSPECIFIED.,.F.,.F.,(4,2,2,2,2,2,
2,2,2,2,2,2,2,2,2,2,2,4),(-84.1468249045191,-84.1043126875934,-83.8659938152791,
-83.6383846593357,-83.4026110967519,-83.1645843112362,-82.9348555875407,
-82.6960900426385,-82.4655136497021,-82.2331702678459,-81.9948224196279,
-81.7671569850544,-81.5321652925085,-81.2914268126568,-81.0623619202666,
-80.8243567680345,-80.5922931190962,-80.3649154835294),.UNSPECIFIED.);
#117=B_SPLINE_CURVE_WITH_KNOTS('',3,(#7437,#7438,#7439,#7440,#7441,#7442,
#7443,#7444,#7445,#7446,#7447,#7448,#7449,#7450,#7451,#7452,#7453,#7454,
#7455,#7456,#7457,#7458,#7459,#7460,#7461,#7462,#7463,#7464,#7465,#7466,
#7467,#7468,#7469,#7470,#7471,#7472),.UNSPECIFIED.,.F.,.F.,(4,2,2,2,2,2,
2,2,2,2,2,2,2,2,2,2,2,4),(-24.2689961176951,-24.0785909762214,-23.8492583670617,
-23.6096469956339,-23.3791830773827,-23.1436638044798,-22.9070380265563,
-22.6790982154573,-22.4407897223783,-22.2069213281478,-21.9785014716679,
-21.7380506822129,-21.5068639881352,-21.2734876567242,-21.0360326284573,
-20.8074498777589,-20.5691549873554,-20.4866764542111),.UNSPECIFIED.);
#118=B_SPLINE_CURVE_WITH_KNOTS('',3,(#7477,#7478,#7479,#7480,#7481,#7482,
#7483,#7484,#7485,#7486,#7487,#7488,#7489,#7490,#7491,#7492,#7493,#7494,
#7495,#7496,#7497,#7498,#7499,#7500,#7501,#7502,#7503,#7504,#7505,#7506,
#7507,#7508,#7509,#7510,#7511,#7512),.UNSPECIFIED.,.F.,.F.,(4,2,2,2,2,2,
2,2,2,2,2,2,2,2,2,2,2,4),(-87.928847460831,-87.846547736004,-87.6082722965554,
-87.3797139714847,-87.142284932425,-86.9089092219722,-86.6777471135071,
-86.4373227129817,-86.208914054241,-85.9750708910875,-85.7367807546045,
-85.5088632525325,-85.2722635629587,-85.036741320696,-84.8063019891483,
-84.5667169550491,-84.3373922845944,-84.1468249045191),.UNSPECIFIED.);
#119=B_SPLINE_CURVE_WITH_KNOTS('',3,(#7513,#7514,#7515,#7516,#7517,#7518,
#7519,#7520,#7521,#7522,#7523,#7524,#7525,#7526,#7527,#7528,#7529,#7530,
#7531,#7532,#7533,#7534,#7535,#7536,#7537,#7538,#7539,#7540,#7541,#7542,
#7543,#7544,#7545,#7546,#7547,#7548),.UNSPECIFIED.,.F.,.F.,(4,2,2,2,2,2,
2,2,2,2,2,2,2,2,2,2,2,4),(-20.4866764542111,-20.3345622966439,-20.1067107417864,
-19.8683346358064,-19.6363719390965,-19.4049599798345,-19.1666234905078,
-18.9372677343282,-18.6977030787119,-18.4623693329401,-18.2347591407509,
-17.9964116855308,-17.7637440061976,-17.5337330948493,-17.2946063174558,
-17.064562599015,-16.8276419602436,-16.7044808578381),.UNSPECIFIED.);
#120=B_SPLINE_CURVE_WITH_KNOTS('',3,(#7553,#7554,#7555,#7556,#7557,#7558,
#7559,#7560,#7561,#7562,#7563,#7564,#7565,#7566,#7567,#7568,#7569,#7570,
#7571,#7572,#7573,#7574,#7575,#7576,#7577,#7578,#7579,#7580,#7581,#7582,
#7583,#7584,#7585,#7586,#7587,#7588),.UNSPECIFIED.,.F.,.F.,(4,2,2,2,2,2,
2,2,2,2,2,2,2,2,2,2,2,4),(-91.7107443282099,-91.5877900079935,-91.3508647690065,
-91.1208457987438,-90.8817454870173,-90.6517409965148,-90.4190984985508,
-90.1807696362717,-89.9531766812327,-89.7178687370554,-89.478297886019,
-89.2489663680631,-89.0106557095446,-88.7792481826981,-88.5473100207957,
-88.3089525160693,-88.0811154260341,-87.928847460831),.UNSPECIFIED.);
#121=B_SPLINE_CURVE_WITH_KNOTS('',3,(#7589,#7590,#7591,#7592,#7593,#7594,
#7595,#7596,#7597,#7598,#7599,#7600,#7601,#7602,#7603,#7604,#7605,#7606,
#7607,#7608,#7609,#7610,#7611,#7612,#7613,#7614,#7615,#7616,#7617,#7618,
#7619,#7620,#7621,#7622,#7623,#7624),.UNSPECIFIED.,.F.,.F.,(4,2,2,2,2,2,
2,2,2,2,2,2,2,2,2,2,2,4),(-16.7044808578381,-16.5915024478014,-16.3637942465863,
-16.1254758543967,-15.8920554985378,-15.6631600972239,-15.4232000339098,
-15.1924359257727,-14.9578801876124,-14.7209079174785,-14.492733046275,
-14.2544426559687,-14.0202587552228,-13.7921192193288,-13.5513242752337,
-13.3198433681694,-13.0872496764959,-12.9221852831127),.UNSPECIFIED.);
#122=B_SPLINE_CURVE_WITH_KNOTS('',3,(#7629,#7630,#7631,#7632,#7633,#7634,
#7635,#7636,#7637,#7638,#7639,#7640,#7641,#7642,#7643,#7644,#7645,#7646,
#7647,#7648,#7649,#7650,#7651,#7652,#7653,#7654,#7655,#7656,#7657,#7658,
#7659,#7660,#7661,#7662,#7663,#7664),.UNSPECIFIED.,.F.,.F.,(4,2,2,2,2,2,
2,2,2,2,2,2,2,2,2,2,2,4),(-95.4927391051041,-95.3278706246628,-95.0952792884395,
-94.8638231831889,-94.6230548711802,-94.394928126947,-94.160769729705,-93.922497949396,
-93.6943470425071,-93.4574011982426,-93.2228439197167,-92.9921047539345,
-92.7521714347657,-92.523285440264,-92.2898906043006,-92.0515908033591,
-91.8239032182906,-91.7107443282099),.UNSPECIFIED.);
#123=B_SPLINE_CURVE_WITH_KNOTS('',3,(#7665,#7666,#7667,#7668,#7669,#7670,
#7671,#7672,#7673,#7674,#7675,#7676,#7677,#7678,#7679,#7680,#7681,#7682,
#7683,#7684,#7685,#7686,#7687,#7688,#7689,#7690,#7691,#7692,#7693,#7694,
#7695,#7696,#7697,#7698,#7699,#7700),.UNSPECIFIED.,.F.,.F.,(4,2,2,2,2,2,
2,2,2,2,2,2,2,2,2,2,2,4),(-12.9221852831127,-12.849459470145,-12.6205816823612,
-12.3822529170638,-12.1473603796708,-11.9196400813886,-11.681270901826,
-11.4490212687812,-11.2182085684104,-10.9795496790003,-10.7499122681144,
-10.5114542542116,-10.275790022471,-10.0481792806899,-9.80983900430133,
-9.57686066008535,-9.34734453006419,-9.1399695593726),.UNSPECIFIED.);
#124=B_SPLINE_CURVE_WITH_KNOTS('',3,(#7707,#7708,#7709,#7710,#7711,#7712,
#7713,#7714,#7715,#7716,#7717,#7718,#7719,#7720,#7721,#7722),
 .UNSPECIFIED.,.F.,.F.,(4,2,2,2,2,2,2,4),(-1.57584202720539,-1.390382595907,
-1.16132802380548,-0.921516936716486,-0.690881872470536,-0.455956835676362,
-0.224750643073495,0.),.UNSPECIFIED.);
#125=B_SPLINE_CURVE_WITH_KNOTS('',3,(#7726,#7727,#7728,#7729,#7730,#7731,
#7732,#7733,#7734,#7735,#7736,#7737,#7738,#7739,#7740,#7741,#7742,#7743),
 .UNSPECIFIED.,.F.,.F.,(4,2,2,2,2,2,2,2,4),(-100.849969952809,-100.666021642914,
-100.475737478142,-100.237444951456,-100.009605932478,-99.7731459818133,
-99.5372345319227,-99.3069163027839,-99.274652338909),.UNSPECIFIED.);
#126=B_SPLINE_CURVE_WITH_KNOTS('',3,(#7746,#7747,#7748,#7749,#7750,#7751,
#7752,#7753,#7754,#7755,#7756,#7757,#7758,#7759,#7760,#7761,#7762,#7763,
#7764,#7765,#7766,#7767,#7768,#7769,#7770,#7771,#7772,#7773,#7774,#7775,
#7776,#7777,#7778,#7779,#7780,#7781),.UNSPECIFIED.,.F.,.F.,(4,2,2,2,2,2,
2,2,2,2,2,2,2,2,2,2,2,4),(-5.35783695894723,-5.13494169831662,-4.90327828502939,
-4.66507524967157,-4.43583667566184,-4.19581412819847,-3.96061776270199,
-3.73299466112997,-3.49464853513548,-3.26211086848107,-3.03188532854683,
-2.79290302357929,-2.56298530835372,-2.32563744780847,-2.08964389026301,
-1.86198435100643,-1.62366727961924,-1.57584202720539),.UNSPECIFIED.);
#127=B_SPLINE_CURVE_WITH_KNOTS('',3,(#7791,#7792,#7793,#7794,#7795,#7796,
#7797,#7798,#7799,#7800,#7801,#7802,#7803,#7804,#7805,#7806,#7807,#7808,
#7809,#7810,#7811,#7812,#7813,#7814,#7815,#7816,#7817,#7818,#7819,#7820,
#7821,#7822,#7823,#7824,#7825,#7826),.UNSPECIFIED.,.F.,.F.,(4,2,2,2,2,2,
2,2,2,2,2,2,2,2,2,2,2,4),(-99.274652338909,-99.0674710790479,-98.8379634210678,
-98.6050102399715,-98.3666888177901,-98.1390968625289,-97.9034584541038,
-97.664996507285,-97.4353834154336,-97.1967504427233,-96.965943920785,-96.733718950633,
-96.495368632197,-96.2676642307138,-96.0327968656458,-95.7944878626794,
-95.5656346615004,-95.4927391051041),.UNSPECIFIED.);
#128=B_SPLINE_CURVE_WITH_KNOTS('',3,(#7827,#7828,#7829,#7830,#7831,#7832,
#7833,#7834,#7835,#7836,#7837,#7838,#7839,#7840,#7841,#7842,#7843,#7844,
#7845,#7846,#7847,#7848,#7849,#7850,#7851,#7852,#7853,#7854,#7855,#7856,
#7857,#7858,#7859,#7860,#7861,#7862,#7863,#7864),.UNSPECIFIED.,.F.,.F.,
(4,2,2,2,2,2,2,2,2,2,2,2,2,2,2,2,2,2,4),(-9.1399695593726,-9.10787291928304,
-8.87753000492313,-8.64162039097332,-8.40513428345374,-8.17727324440492,
-7.93896185891339,-7.7052216609661,-7.47667817446303,-7.23636744989055,
-7.00530119291182,-6.77160155078404,-6.5342837597148,-6.30582239728129,
-6.06754425945498,-5.83307490876647,-5.60516032837488,-5.36678566314923,
-5.35783695894723),.UNSPECIFIED.);
#129=B_SPLINE_CURVE_WITH_KNOTS('',3,(#11058,#11059,#11060,#11061,#11062,
#11063,#11064,#11065,#11066,#11067,#11068,#11069,#11070,#11071,#11072,#11073,
#11074,#11075,#11076,#11077),.UNSPECIFIED.,.F.,.F.,(4,2,2,2,2,2,2,2,2,4),
(0.,0.192262276611165,0.36487527397464,0.666841526039601,0.859077160205319,
0.933919508034091,0.964372101203401,0.976575083217201,0.981856483830181,
0.986854022611611),.UNSPECIFIED.);
#130=B_SPLINE_CURVE_WITH_KNOTS('',3,(#13254,#13255,#13256,#13257,#13258,
#13259,#13260,#13261,#13262,#13263,#13264,#13265,#13266,#13267,#13268,#13269,
#13270,#13271,#13272,#13273),.UNSPECIFIED.,.F.,.F.,(4,2,2,2,2,2,2,2,2,4),
(1.00001729274522E-6,0.000806658582909784,0.00167003986182473,0.00372333846850495,
0.00950633881409832,0.0259676755535791,0.0679386431653802,0.119530949671773,
0.1558134434742,0.196417574801726),.UNSPECIFIED.);
#131=B_SPLINE_CURVE_WITH_KNOTS('',3,(#13305,#13306,#13307,#13308,#13309,
#13310),.UNSPECIFIED.,.F.,.F.,(4,2,4),(0.00553837226488889,0.00830239406258802,
0.0110664158602872),.UNSPECIFIED.);
#132=B_SPLINE_CURVE_WITH_KNOTS('',3,(#13312,#13313,#13314,#13315,#13316,
#13317,#13318,#13319,#13320,#13321),.UNSPECIFIED.,.F.,.F.,(4,2,2,2,4),(0.,
0.00276660396507179,0.00553320793014358,0.00829981189521537,0.0110664158602872),
 .UNSPECIFIED.);
#133=B_SPLINE_CURVE_WITH_KNOTS('',3,(#13323,#13324,#13325,#13326,#13327,
#13328,#13329,#13330,#13331,#13332),.UNSPECIFIED.,.F.,.F.,(4,2,2,2,4),(1.62072509839964E-19,
0.00276660396507179,0.00553320793014358,0.00829981189521537,0.0110664158602872),
 .UNSPECIFIED.);
#134=B_SPLINE_CURVE_WITH_KNOTS('',3,(#13334,#13335,#13336,#13337,#13338,
#13339,#13340,#13341,#13342,#13343,#13344,#13345,#13346,#13347,#13348,#13349,
#13350,#13351,#13352,#13353,#13354,#13355),.UNSPECIFIED.,.F.,.F.,(4,3,3,
3,3,3,3,4),(0.,0.00114977203808909,0.00217838054954922,0.00274980879509083,
0.00276918613244445,0.00408374644507523,0.00535443888579874,0.0055383722648889),
 .UNSPECIFIED.);
#135=B_SPLINE_CURVE_WITH_KNOTS('',3,(#13357,#13358,#13359,#13360,#13361,
#13362),.UNSPECIFIED.,.F.,.F.,(4,2,4),(0.0055383722648889,0.00830239406258803,
0.0110664158602872),.UNSPECIFIED.);
#136=B_SPLINE_CURVE_WITH_KNOTS('',3,(#13364,#13365,#13366,#13367,#13368,
#13369,#13370,#13371,#13372,#13373),.UNSPECIFIED.,.F.,.F.,(4,2,2,2,4),(0.,
0.00276660396507179,0.00553320793014358,0.00829981189521537,0.0110664158602872),
 .UNSPECIFIED.);
#137=B_SPLINE_CURVE_WITH_KNOTS('',3,(#13375,#13376,#13377,#13378,#13379,
#13380,#13381,#13382,#13383,#13384),.UNSPECIFIED.,.F.,.F.,(4,2,2,2,4),(0.,
0.00276660396507179,0.00553320793014358,0.00829981189521537,0.0110664158602872),
 .UNSPECIFIED.);
#138=B_SPLINE_CURVE_WITH_KNOTS('',3,(#13385,#13386,#13387,#13388,#13389,
#13390),.UNSPECIFIED.,.F.,.F.,(4,2,4),(0.,0.00276918613244445,0.00553837226488889),
 .UNSPECIFIED.);
#139=B_SPLINE_CURVE_WITH_KNOTS('',3,(#13403,#13404,#13405,#13406,#13407,
#13408,#13409,#13410,#13411,#13412,#13413,#13414,#13415,#13416,#13417,#13418,
#13419,#13420,#13421,#13422,#13423,#13424,#13425,#13426,#13427,#13428,#13429,
#13430,#13431,#13432,#13433,#13434,#13435,#13436,#13437,#13438,#13439),
 .UNSPECIFIED.,.F.,.F.,(4,3,3,3,3,3,3,3,3,3,3,3,4),(0.,0.00104332150239121,
0.00206065848340059,0.00259807621135332,0.00371876749530484,0.00484862102586553,
0.00515636113902887,0.00519615242270663,0.00700298769703306,0.00779422863405995,
0.00803596165391469,0.00922538326593667,0.0103923048454133),
 .UNSPECIFIED.);
#140=B_SPLINE_CURVE_WITH_KNOTS('',3,(#13453,#13454,#13455,#13456,#13457,
#13458,#13459,#13460,#13461,#13462,#13463,#13464,#13465,#13466,#13467,#13468,
#13469,#13470,#13471,#13472,#13473,#13474,#13475,#13476,#13477,#13478,#13479,
#13480,#13481,#13482,#13483,#13484,#13485,#13486,#13487,#13488,#13489),
 .UNSPECIFIED.,.F.,.F.,(4,3,3,3,3,3,3,3,3,3,3,3,4),(0.,0.00104332150241254,
0.00206065848345604,0.00259807621135332,0.00371876749530863,0.00484862102596152,
0.00515636113902889,0.00519615242270663,0.00700298769762406,0.00779422863405995,
0.00803596165391469,0.00922538326592427,0.0103923048454133),
 .UNSPECIFIED.);
#141=B_SPLINE_CURVE_WITH_KNOTS('',3,(#13501,#13502,#13503,#13504,#13505,
#13506,#13507,#13508,#13509,#13510,#13511,#13512,#13513,#13514,#13515,#13516,
#13517,#13518,#13519,#13520,#13521,#13522,#13523,#13524,#13525,#13526,#13527,
#13528,#13529,#13530,#13531,#13532,#13533,#13534,#13535,#13536,#13537),
 .UNSPECIFIED.,.F.,.F.,(4,3,3,3,3,3,3,3,3,3,3,3,4),(0.,0.00104353079945368,
0.0020610675491746,0.00259807621135332,0.00371858000064792,0.00484809657734561,
0.00515608341291941,0.00519615242270663,0.00716112156284184,0.00779422863405995,
0.00803585117301137,0.00922121712355728,0.0103923048454133),
 .UNSPECIFIED.);
#142=B_SPLINE_CURVE_WITH_KNOTS('',3,(#13549,#13550,#13551,#13552,#13553,
#13554,#13555,#13556,#13557,#13558,#13559,#13560,#13561,#13562,#13563,#13564,
#13565,#13566,#13567,#13568,#13569,#13570,#13571,#13572,#13573,#13574,#13575,
#13576,#13577,#13578,#13579,#13580,#13581,#13582,#13583,#13584,#13585),
 .UNSPECIFIED.,.F.,.F.,(4,3,3,3,3,3,3,3,3,3,3,3,4),(0.,0.00104332150237409,
0.00206065848338429,0.00259807621135332,0.00371876749530815,0.00484862102586396,
0.00515636113902887,0.00519615242270663,0.00700298769768474,0.00779422863405995,
0.0080359616539147,0.00922538326598745,0.0103923048454133),
 .UNSPECIFIED.);
#143=B_SPLINE_CURVE_WITH_KNOTS('',3,(#13597,#13598,#13599,#13600,#13601,
#13602,#13603,#13604,#13605,#13606,#13607,#13608,#13609,#13610,#13611,#13612,
#13613,#13614,#13615,#13616,#13617,#13618,#13619,#13620,#13621,#13622,#13623,
#13624,#13625,#13626,#13627,#13628,#13629,#13630,#13631,#13632,#13633),
 .UNSPECIFIED.,.F.,.F.,(4,3,3,3,3,3,3,3,3,3,3,3,4),(0.,0.001043321502395,
0.00206065848341437,0.00259807621135332,0.00371876749539627,0.00484862102602629,
0.00515636113902888,0.00519615242270663,0.00700298769718223,0.00779422863405995,
0.00803596165391469,0.00922538326593071,0.0103923048454133),
 .UNSPECIFIED.);
#144=B_SPLINE_CURVE_WITH_KNOTS('',3,(#13642,#13643,#13644,#13645,#13646,
#13647,#13648,#13649,#13650,#13651,#13652,#13653,#13654,#13655,#13656,#13657,
#13658,#13659,#13660,#13661,#13662,#13663,#13664,#13665,#13666,#13667,#13668,
#13669,#13670,#13671,#13672,#13673,#13674,#13675,#13676,#13677,#13678),
 .UNSPECIFIED.,.F.,.F.,(4,3,3,3,3,3,3,3,3,3,3,3,4),(0.,0.0010434213010507,
0.00206085463009113,0.00259807621135332,0.0037190935981022,0.0048493549766946,
0.0051567201755677,0.00519615242270663,0.00684590372399744,0.00779422863405995,
0.00803611110738811,0.009229743876539,0.0103923048454133),.UNSPECIFIED.);
#145=B_SPLINE_CURVE_WITH_KNOTS('',3,(#13724,#13725,#13726,#13727,#13728,
#13729,#13730,#13731,#13732,#13733,#13734,#13735,#13736,#13737,#13738,#13739,
#13740,#13741,#13742,#13743,#13744,#13745,#13746,#13747,#13748,#13749,#13750,
#13751,#13752,#13753,#13754),.UNSPECIFIED.,.F.,.F.,(4,3,3,3,3,3,3,3,3,3,
4),(-5.63655962566362E-6,0.000138968027467558,0.000300786513285965,0.000418320464104159,
0.000498923906492782,0.000607102007354961,0.000706192487495778,0.000797150264455975,
0.000884559431233306,0.00096812822464727,0.00100346392791823),
 .UNSPECIFIED.);
#146=B_SPLINE_CURVE_WITH_KNOTS('',3,(#13755,#13756,#13757,#13758,#13759,
#13760,#13761,#13762,#13763,#13764,#13765,#13766,#13767,#13768,#13769,#13770,
#13771,#13772,#13773,#13774,#13775,#13776,#13777,#13778,#13779,#13780,#13781,
#13782,#13783,#13784,#13785),.UNSPECIFIED.,.F.,.F.,(4,3,3,3,3,3,3,3,3,3,
4),(2.03723854135766E-8,8.34362348219312E-5,0.000169714573606459,0.000262192398767452,
0.000359257400005965,0.000466160307363708,0.000502785923637984,0.000616382138541576,
0.0007569494209109,0.000924038166163904,0.00100557184727597),
 .UNSPECIFIED.);
#147=B_SPLINE_CURVE_WITH_KNOTS('',3,(#13810,#13811,#13812,#13813,#13814,
#13815,#13816,#13817,#13818,#13819,#13820,#13821,#13822,#13823,#13824,#13825,
#13826,#13827,#13828,#13829,#13830,#13831,#13832,#13833,#13834,#13835,#13836,
#13837,#13838,#13839,#13840),.UNSPECIFIED.,.F.,.F.,(4,3,3,3,3,3,3,3,3,3,
4),(2.03923073170011E-8,8.34362553594438E-5,0.000169714594923251,0.000262192421030851,
0.000359257423499574,0.000466160332015168,0.000502785923637989,0.000616382138542073,
0.000756949420907432,0.000924038166154207,0.00100557184727598),
 .UNSPECIFIED.);
#148=B_SPLINE_CURVE_WITH_KNOTS('',3,(#13865,#13866,#13867,#13868,#13869,
#13870,#13871,#13872,#13873,#13874,#13875,#13876,#13877,#13878,#13879,#13880,
#13881,#13882,#13883,#13884,#13885,#13886,#13887,#13888,#13889,#13890,#13891,
#13892,#13893,#13894,#13895),.UNSPECIFIED.,.F.,.F.,(4,3,3,3,3,3,3,3,3,3,
4),(-5.63655962566659E-6,0.000138967995190904,0.000300786409144175,0.00041832036912045,
0.00049892390649278,0.000607102001454561,0.000706192477737142,0.000797150254787515,
0.000884559421701961,0.000968128215167521,0.00100346390658489),
 .UNSPECIFIED.);
#149=B_SPLINE_CURVE_WITH_KNOTS('',3,(#13920,#13921,#13922,#13923,#13924,
#13925,#13926,#13927,#13928,#13929,#13930,#13931,#13932,#13933,#13934,#13935,
#13936,#13937,#13938,#13939,#13940,#13941,#13942,#13943,#13944,#13945,#13946,
#13947,#13948,#13949,#13950),.UNSPECIFIED.,.F.,.F.,(4,3,3,3,3,3,3,3,3,3,
4),(2.03723849519033E-8,8.34362343361756E-5,0.000169714572665549,0.000262192396983797,
0.000359257396479951,0.000466160298033514,0.00050278592363799,0.000616382140865371,
0.000756949409341133,0.000924038066230108,0.00100557184727598),
 .UNSPECIFIED.);
#150=B_SPLINE_CURVE_WITH_KNOTS('',3,(#13975,#13976,#13977,#13978,#13979,
#13980,#13981,#13982,#13983,#13984,#13985,#13986,#13987,#13988,#13989,#13990,
#13991,#13992,#13993,#13994,#13995,#13996,#13997,#13998,#13999,#14000,#14001,
#14002,#14003,#14004,#14005),.UNSPECIFIED.,.F.,.F.,(4,3,3,3,3,3,3,3,3,3,
4),(-5.63655962566647E-6,0.000138967995317118,0.00030078640930236,0.000418320369284012,
0.000498923906492781,0.000607102001183047,0.000706192482866764,0.000797150259424217,
0.000884559425945727,0.000968128218988905,0.00100346392791791),
 .UNSPECIFIED.);
#151=(
BOUNDED_CURVE()
B_SPLINE_CURVE(2,(#5000,#5001,#5002),.UNSPECIFIED.,.F.,.F.)
B_SPLINE_CURVE_WITH_KNOTS((3,3),(0.981481481481482,0.987654320987654),
 .UNSPECIFIED.)
CURVE()
GEOMETRIC_REPRESENTATION_ITEM()
RATIONAL_B_SPLINE_CURVE((1.,0.866025403784439,1.))
REPRESENTATION_ITEM('')
);
#152=(
BOUNDED_CURVE()
B_SPLINE_CURVE(2,(#5005,#5006,#5007),.UNSPECIFIED.,.F.,.F.)
B_SPLINE_CURVE_WITH_KNOTS((3,3),(0.981481481481482,0.987654320987654),
 .UNSPECIFIED.)
CURVE()
GEOMETRIC_REPRESENTATION_ITEM()
RATIONAL_B_SPLINE_CURVE((1.,0.866025403784439,1.))
REPRESENTATION_ITEM('')
);
#153=(
BOUNDED_CURVE()
B_SPLINE_CURVE(2,(#5012,#5013,#5014,#5015,#5016,#5017,#5018,#5019,#5020,
#5021,#5022,#5023,#5024),.UNSPECIFIED.,.F.,.F.)
B_SPLINE_CURVE_WITH_KNOTS((3,2,2,2,2,2,3),(0.944444444444444,0.950617283950617,
0.95679012345679,0.962962962962963,0.969135802469136,0.975308641975309,
0.981481481481482),.UNSPECIFIED.)
CURVE()
GEOMETRIC_REPRESENTATION_ITEM()
RATIONAL_B_SPLINE_CURVE((1.,0.866025403784439,1.,0.866025403784439,1.,0.866025403784439,
1.,0.866025403784439,1.,0.866025403784439,1.,0.866025403784439,1.))
REPRESENTATION_ITEM('')
);
#154=(
BOUNDED_CURVE()
B_SPLINE_CURVE(2,(#5025,#5026,#5027,#5028,#5029,#5030,#5031,#5032,#5033,
#5034,#5035,#5036,#5037),.UNSPECIFIED.,.F.,.F.)
B_SPLINE_CURVE_WITH_KNOTS((3,2,2,2,2,2,3),(0.944444444444444,0.950617283950617,
0.95679012345679,0.962962962962963,0.969135802469136,0.975308641975309,
0.981481481481482),.UNSPECIFIED.)
CURVE()
GEOMETRIC_REPRESENTATION_ITEM()
RATIONAL_B_SPLINE_CURVE((1.,0.866025403784439,1.,0.866025403784439,1.,0.866025403784439,
1.,0.866025403784439,1.,0.866025403784439,1.,0.866025403784439,1.))
REPRESENTATION_ITEM('')
);
#155=(
BOUNDED_CURVE()
B_SPLINE_CURVE(2,(#5042,#5043,#5044,#5045,#5046,#5047,#5048,#5049,#5050,
#5051,#5052,#5053,#5054),.UNSPECIFIED.,.F.,.F.)
B_SPLINE_CURVE_WITH_KNOTS((3,2,2,2,2,2,3),(0.907407407407407,0.91358024691358,
0.919753086419753,0.925925925925926,0.932098765432099,0.938271604938272,
0.944444444444444),.UNSPECIFIED.)
CURVE()
GEOMETRIC_REPRESENTATION_ITEM()
RATIONAL_B_SPLINE_CURVE((1.,0.866025403784439,1.,0.866025403784439,1.,0.866025403784439,
1.,0.866025403784439,1.,0.866025403784439,1.,0.866025403784439,1.))
REPRESENTATION_ITEM('')
);
#156=(
BOUNDED_CURVE()
B_SPLINE_CURVE(2,(#5055,#5056,#5057,#5058,#5059,#5060,#5061,#5062,#5063,
#5064,#5065,#5066,#5067),.UNSPECIFIED.,.F.,.F.)
B_SPLINE_CURVE_WITH_KNOTS((3,2,2,2,2,2,3),(0.907407407407407,0.91358024691358,
0.919753086419753,0.925925925925926,0.932098765432099,0.938271604938272,
0.944444444444444),.UNSPECIFIED.)
CURVE()
GEOMETRIC_REPRESENTATION_ITEM()
RATIONAL_B_SPLINE_CURVE((1.,0.866025403784439,1.,0.866025403784439,1.,0.866025403784439,
1.,0.866025403784439,1.,0.866025403784439,1.,0.866025403784439,1.))
REPRESENTATION_ITEM('')
);
#157=(
BOUNDED_CURVE()
B_SPLINE_CURVE(2,(#5072,#5073,#5074,#5075,#5076,#5077,#5078,#5079,#5080,
#5081,#5082,#5083,#5084),.UNSPECIFIED.,.F.,.F.)
B_SPLINE_CURVE_WITH_KNOTS((3,2,2,2,2,2,3),(0.87037037037037,0.876543209876543,
0.882716049382716,0.888888888888889,0.895061728395062,0.901234567901235,
0.907407407407407),.UNSPECIFIED.)
CURVE()
GEOMETRIC_REPRESENTATION_ITEM()
RATIONAL_B_SPLINE_CURVE((1.,0.866025403784439,1.,0.866025403784439,1.,0.866025403784439,
1.,0.866025403784439,1.,0.866025403784439,1.,0.866025403784439,1.))
REPRESENTATION_ITEM('')
);
#158=(
BOUNDED_CURVE()
B_SPLINE_CURVE(2,(#5085,#5086,#5087,#5088,#5089,#5090,#5091,#5092,#5093,
#5094,#5095,#5096,#5097),.UNSPECIFIED.,.F.,.F.)
B_SPLINE_CURVE_WITH_KNOTS((3,2,2,2,2,2,3),(0.87037037037037,0.876543209876543,
0.882716049382716,0.888888888888889,0.895061728395062,0.901234567901235,
0.907407407407407),.UNSPECIFIED.)
CURVE()
GEOMETRIC_REPRESENTATION_ITEM()
RATIONAL_B_SPLINE_CURVE((1.,0.866025403784439,1.,0.866025403784439,1.,0.866025403784439,
1.,0.866025403784439,1.,0.866025403784439,1.,0.866025403784439,1.))
REPRESENTATION_ITEM('')
);
#159=(
BOUNDED_CURVE()
B_SPLINE_CURVE(2,(#5102,#5103,#5104,#5105,#5106,#5107,#5108,#5109,#5110,
#5111,#5112,#5113,#5114),.UNSPECIFIED.,.F.,.F.)
B_SPLINE_CURVE_WITH_KNOTS((3,2,2,2,2,2,3),(0.833333333333333,0.839506172839506,
0.845679012345679,0.851851851851852,0.858024691358025,0.864197530864197,
0.87037037037037),.UNSPECIFIED.)
CURVE()
GEOMETRIC_REPRESENTATION_ITEM()
RATIONAL_B_SPLINE_CURVE((1.,0.866025403784439,1.,0.866025403784439,1.,0.866025403784439,
1.,0.866025403784439,1.,0.866025403784439,1.,0.866025403784439,1.))
REPRESENTATION_ITEM('')
);
#160=(
BOUNDED_CURVE()
B_SPLINE_CURVE(2,(#5115,#5116,#5117,#5118,#5119,#5120,#5121,#5122,#5123,
#5124,#5125,#5126,#5127),.UNSPECIFIED.,.F.,.F.)
B_SPLINE_CURVE_WITH_KNOTS((3,2,2,2,2,2,3),(0.833333333333333,0.839506172839506,
0.845679012345679,0.851851851851852,0.858024691358025,0.864197530864197,
0.87037037037037),.UNSPECIFIED.)
CURVE()
GEOMETRIC_REPRESENTATION_ITEM()
RATIONAL_B_SPLINE_CURVE((1.,0.866025403784439,1.,0.866025403784439,1.,0.866025403784439,
1.,0.866025403784439,1.,0.866025403784439,1.,0.866025403784439,1.))
REPRESENTATION_ITEM('')
);
#161=(
BOUNDED_CURVE()
B_SPLINE_CURVE(2,(#5132,#5133,#5134,#5135,#5136,#5137,#5138,#5139,#5140,
#5141,#5142,#5143,#5144),.UNSPECIFIED.,.F.,.F.)
B_SPLINE_CURVE_WITH_KNOTS((3,2,2,2,2,2,3),(0.796296296296296,0.802469135802469,
0.808641975308642,0.814814814814815,0.820987654320988,0.827160493827161,
0.833333333333333),.UNSPECIFIED.)
CURVE()
GEOMETRIC_REPRESENTATION_ITEM()
RATIONAL_B_SPLINE_CURVE((1.,0.866025403784439,1.,0.866025403784439,1.,0.866025403784439,
1.,0.866025403784439,1.,0.866025403784439,1.,0.866025403784439,1.))
REPRESENTATION_ITEM('')
);
#162=(
BOUNDED_CURVE()
B_SPLINE_CURVE(2,(#5145,#5146,#5147,#5148,#5149,#5150,#5151,#5152,#5153,
#5154,#5155,#5156,#5157),.UNSPECIFIED.,.F.,.F.)
B_SPLINE_CURVE_WITH_KNOTS((3,2,2,2,2,2,3),(0.796296296296296,0.802469135802469,
0.808641975308642,0.814814814814815,0.820987654320988,0.827160493827161,
0.833333333333333),.UNSPECIFIED.)
CURVE()
GEOMETRIC_REPRESENTATION_ITEM()
RATIONAL_B_SPLINE_CURVE((1.,0.866025403784439,1.,0.866025403784439,1.,0.866025403784439,
1.,0.866025403784439,1.,0.866025403784439,1.,0.866025403784439,1.))
REPRESENTATION_ITEM('')
);
#163=(
BOUNDED_CURVE()
B_SPLINE_CURVE(2,(#5162,#5163,#5164,#5165,#5166,#5167,#5168,#5169,#5170,
#5171,#5172,#5173,#5174),.UNSPECIFIED.,.F.,.F.)
B_SPLINE_CURVE_WITH_KNOTS((3,2,2,2,2,2,3),(0.759259259259259,0.765432098765432,
0.771604938271605,0.777777777777778,0.783950617283951,0.790123456790123,
0.796296296296296),.UNSPECIFIED.)
CURVE()
GEOMETRIC_REPRESENTATION_ITEM()
RATIONAL_B_SPLINE_CURVE((1.,0.866025403784439,1.,0.866025403784439,1.,0.866025403784439,
1.,0.866025403784439,1.,0.866025403784439,1.,0.866025403784439,1.))
REPRESENTATION_ITEM('')
);
#164=(
BOUNDED_CURVE()
B_SPLINE_CURVE(2,(#5175,#5176,#5177,#5178,#5179,#5180,#5181,#5182,#5183,
#5184,#5185,#5186,#5187),.UNSPECIFIED.,.F.,.F.)
B_SPLINE_CURVE_WITH_KNOTS((3,2,2,2,2,2,3),(0.759259259259259,0.765432098765432,
0.771604938271605,0.777777777777778,0.783950617283951,0.790123456790123,
0.796296296296296),.UNSPECIFIED.)
CURVE()
GEOMETRIC_REPRESENTATION_ITEM()
RATIONAL_B_SPLINE_CURVE((1.,0.866025403784439,1.,0.866025403784439,1.,0.866025403784439,
1.,0.866025403784439,1.,0.866025403784439,1.,0.866025403784439,1.))
REPRESENTATION_ITEM('')
);
#165=(
BOUNDED_CURVE()
B_SPLINE_CURVE(2,(#5192,#5193,#5194,#5195,#5196,#5197,#5198,#5199,#5200,
#5201,#5202,#5203,#5204),.UNSPECIFIED.,.F.,.F.)
B_SPLINE_CURVE_WITH_KNOTS((3,2,2,2,2,2,3),(0.722222222222222,0.728395061728395,
0.734567901234568,0.740740740740741,0.746913580246914,0.753086419753086,
0.759259259259259),.UNSPECIFIED.)
CURVE()
GEOMETRIC_REPRESENTATION_ITEM()
RATIONAL_B_SPLINE_CURVE((1.,0.866025403784439,1.,0.866025403784439,1.,0.866025403784439,
1.,0.866025403784439,1.,0.866025403784439,1.,0.866025403784439,1.))
REPRESENTATION_ITEM('')
);
#166=(
BOUNDED_CURVE()
B_SPLINE_CURVE(2,(#5205,#5206,#5207,#5208,#5209,#5210,#5211,#5212,#5213,
#5214,#5215,#5216,#5217),.UNSPECIFIED.,.F.,.F.)
B_SPLINE_CURVE_WITH_KNOTS((3,2,2,2,2,2,3),(0.722222222222222,0.728395061728395,
0.734567901234568,0.740740740740741,0.746913580246914,0.753086419753086,
0.759259259259259),.UNSPECIFIED.)
CURVE()
GEOMETRIC_REPRESENTATION_ITEM()
RATIONAL_B_SPLINE_CURVE((1.,0.866025403784439,1.,0.866025403784439,1.,0.866025403784439,
1.,0.866025403784439,1.,0.866025403784439,1.,0.866025403784439,1.))
REPRESENTATION_ITEM('')
);
#167=(
BOUNDED_CURVE()
B_SPLINE_CURVE(2,(#5222,#5223,#5224,#5225,#5226,#5227,#5228,#5229,#5230,
#5231,#5232,#5233,#5234),.UNSPECIFIED.,.F.,.F.)
B_SPLINE_CURVE_WITH_KNOTS((3,2,2,2,2,2,3),(0.685185185185185,0.691358024691358,
0.697530864197531,0.703703703703704,0.709876543209877,0.716049382716049,
0.722222222222222),.UNSPECIFIED.)
CURVE()
GEOMETRIC_REPRESENTATION_ITEM()
RATIONAL_B_SPLINE_CURVE((1.,0.866025403784439,1.,0.866025403784439,1.,0.866025403784439,
1.,0.866025403784439,1.,0.866025403784439,1.,0.866025403784439,1.))
REPRESENTATION_ITEM('')
);
#168=(
BOUNDED_CURVE()
B_SPLINE_CURVE(2,(#5235,#5236,#5237,#5238,#5239,#5240,#5241,#5242,#5243,
#5244,#5245,#5246,#5247),.UNSPECIFIED.,.F.,.F.)
B_SPLINE_CURVE_WITH_KNOTS((3,2,2,2,2,2,3),(0.685185185185185,0.691358024691358,
0.697530864197531,0.703703703703704,0.709876543209877,0.716049382716049,
0.722222222222222),.UNSPECIFIED.)
CURVE()
GEOMETRIC_REPRESENTATION_ITEM()
RATIONAL_B_SPLINE_CURVE((1.,0.866025403784439,1.,0.866025403784439,1.,0.866025403784439,
1.,0.866025403784439,1.,0.866025403784439,1.,0.866025403784439,1.))
REPRESENTATION_ITEM('')
);
#169=(
BOUNDED_CURVE()
B_SPLINE_CURVE(2,(#5252,#5253,#5254,#5255,#5256,#5257,#5258,#5259,#5260,
#5261,#5262,#5263,#5264),.UNSPECIFIED.,.F.,.F.)
B_SPLINE_CURVE_WITH_KNOTS((3,2,2,2,2,2,3),(0.648148148148148,0.654320987654321,
0.660493827160494,0.666666666666667,0.672839506172839,0.679012345679012,
0.685185185185185),.UNSPECIFIED.)
CURVE()
GEOMETRIC_REPRESENTATION_ITEM()
RATIONAL_B_SPLINE_CURVE((1.,0.866025403784439,1.,0.866025403784439,1.,0.866025403784439,
1.,0.866025403784439,1.,0.866025403784439,1.,0.866025403784439,1.))
REPRESENTATION_ITEM('')
);
#170=(
BOUNDED_CURVE()
B_SPLINE_CURVE(2,(#5265,#5266,#5267,#5268,#5269,#5270,#5271,#5272,#5273,
#5274,#5275,#5276,#5277),.UNSPECIFIED.,.F.,.F.)
B_SPLINE_CURVE_WITH_KNOTS((3,2,2,2,2,2,3),(0.648148148148148,0.654320987654321,
0.660493827160494,0.666666666666667,0.672839506172839,0.679012345679012,
0.685185185185185),.UNSPECIFIED.)
CURVE()
GEOMETRIC_REPRESENTATION_ITEM()
RATIONAL_B_SPLINE_CURVE((1.,0.866025403784439,1.,0.866025403784439,1.,0.866025403784439,
1.,0.866025403784439,1.,0.866025403784439,1.,0.866025403784439,1.))
REPRESENTATION_ITEM('')
);
#171=(
BOUNDED_CURVE()
B_SPLINE_CURVE(2,(#5282,#5283,#5284,#5285,#5286,#5287,#5288,#5289,#5290,
#5291,#5292,#5293,#5294),.UNSPECIFIED.,.F.,.F.)
B_SPLINE_CURVE_WITH_KNOTS((3,2,2,2,2,2,3),(0.611111111111111,0.617283950617284,
0.623456790123457,0.62962962962963,0.635802469135803,0.641975308641975,
0.648148148148148),.UNSPECIFIED.)
CURVE()
GEOMETRIC_REPRESENTATION_ITEM()
RATIONAL_B_SPLINE_CURVE((1.,0.866025403784439,1.,0.866025403784439,1.,0.866025403784439,
1.,0.866025403784439,1.,0.866025403784439,1.,0.866025403784439,1.))
REPRESENTATION_ITEM('')
);
#172=(
BOUNDED_CURVE()
B_SPLINE_CURVE(2,(#5295,#5296,#5297,#5298,#5299,#5300,#5301,#5302,#5303,
#5304,#5305,#5306,#5307),.UNSPECIFIED.,.F.,.F.)
B_SPLINE_CURVE_WITH_KNOTS((3,2,2,2,2,2,3),(0.611111111111111,0.617283950617284,
0.623456790123457,0.62962962962963,0.635802469135803,0.641975308641975,
0.648148148148148),.UNSPECIFIED.)
CURVE()
GEOMETRIC_REPRESENTATION_ITEM()
RATIONAL_B_SPLINE_CURVE((1.,0.866025403784439,1.,0.866025403784439,1.,0.866025403784439,
1.,0.866025403784439,1.,0.866025403784439,1.,0.866025403784439,1.))
REPRESENTATION_ITEM('')
);
#173=(
BOUNDED_CURVE()
B_SPLINE_CURVE(2,(#5312,#5313,#5314,#5315,#5316,#5317,#5318,#5319,#5320,
#5321,#5322,#5323,#5324),.UNSPECIFIED.,.F.,.F.)
B_SPLINE_CURVE_WITH_KNOTS((3,2,2,2,2,2,3),(0.574074074074074,0.580246913580247,
0.58641975308642,0.592592592592593,0.598765432098765,0.604938271604938,
0.611111111111111),.UNSPECIFIED.)
CURVE()
GEOMETRIC_REPRESENTATION_ITEM()
RATIONAL_B_SPLINE_CURVE((1.,0.866025403784439,1.,0.866025403784439,1.,0.866025403784439,
1.,0.866025403784439,1.,0.866025403784439,1.,0.866025403784439,1.))
REPRESENTATION_ITEM('')
);
#174=(
BOUNDED_CURVE()
B_SPLINE_CURVE(2,(#5325,#5326,#5327,#5328,#5329,#5330,#5331,#5332,#5333,
#5334,#5335,#5336,#5337),.UNSPECIFIED.,.F.,.F.)
B_SPLINE_CURVE_WITH_KNOTS((3,2,2,2,2,2,3),(0.574074074074074,0.580246913580247,
0.58641975308642,0.592592592592593,0.598765432098765,0.604938271604938,
0.611111111111111),.UNSPECIFIED.)
CURVE()
GEOMETRIC_REPRESENTATION_ITEM()
RATIONAL_B_SPLINE_CURVE((1.,0.866025403784439,1.,0.866025403784439,1.,0.866025403784439,
1.,0.866025403784439,1.,0.866025403784439,1.,0.866025403784439,1.))
REPRESENTATION_ITEM('')
);
#175=(
BOUNDED_CURVE()
B_SPLINE_CURVE(2,(#5342,#5343,#5344,#5345,#5346,#5347,#5348,#5349,#5350,
#5351,#5352,#5353,#5354),.UNSPECIFIED.,.F.,.F.)
B_SPLINE_CURVE_WITH_KNOTS((3,2,2,2,2,2,3),(0.537037037037037,0.54320987654321,
0.549382716049383,0.555555555555556,0.561728395061728,0.567901234567901,
0.574074074074074),.UNSPECIFIED.)
CURVE()
GEOMETRIC_REPRESENTATION_ITEM()
RATIONAL_B_SPLINE_CURVE((1.,0.866025403784439,1.,0.866025403784439,1.,0.866025403784439,
1.,0.866025403784439,1.,0.866025403784439,1.,0.866025403784439,1.))
REPRESENTATION_ITEM('')
);
#176=(
BOUNDED_CURVE()
B_SPLINE_CURVE(2,(#5355,#5356,#5357,#5358,#5359,#5360,#5361,#5362,#5363,
#5364,#5365,#5366,#5367),.UNSPECIFIED.,.F.,.F.)
B_SPLINE_CURVE_WITH_KNOTS((3,2,2,2,2,2,3),(0.537037037037037,0.54320987654321,
0.549382716049383,0.555555555555556,0.561728395061728,0.567901234567901,
0.574074074074074),.UNSPECIFIED.)
CURVE()
GEOMETRIC_REPRESENTATION_ITEM()
RATIONAL_B_SPLINE_CURVE((1.,0.866025403784439,1.,0.866025403784439,1.,0.866025403784439,
1.,0.866025403784439,1.,0.866025403784439,1.,0.866025403784439,1.))
REPRESENTATION_ITEM('')
);
#177=(
BOUNDED_CURVE()
B_SPLINE_CURVE(2,(#5372,#5373,#5374,#5375,#5376,#5377,#5378,#5379,#5380,
#5381,#5382,#5383,#5384),.UNSPECIFIED.,.F.,.F.)
B_SPLINE_CURVE_WITH_KNOTS((3,2,2,2,2,2,3),(0.5,0.506172839506173,0.512345679012346,
0.518518518518518,0.524691358024691,0.530864197530864,0.537037037037037),
 .UNSPECIFIED.)
CURVE()
GEOMETRIC_REPRESENTATION_ITEM()
RATIONAL_B_SPLINE_CURVE((1.,0.866025403784439,1.,0.866025403784439,1.,0.866025403784439,
1.,0.866025403784439,1.,0.866025403784439,1.,0.866025403784439,1.))
REPRESENTATION_ITEM('')
);
#178=(
BOUNDED_CURVE()
B_SPLINE_CURVE(2,(#5385,#5386,#5387,#5388,#5389,#5390,#5391,#5392,#5393,
#5394,#5395,#5396,#5397),.UNSPECIFIED.,.F.,.F.)
B_SPLINE_CURVE_WITH_KNOTS((3,2,2,2,2,2,3),(0.5,0.506172839506173,0.512345679012346,
0.518518518518518,0.524691358024691,0.530864197530864,0.537037037037037),
 .UNSPECIFIED.)
CURVE()
GEOMETRIC_REPRESENTATION_ITEM()
RATIONAL_B_SPLINE_CURVE((1.,0.866025403784439,1.,0.866025403784439,1.,0.866025403784439,
1.,0.866025403784439,1.,0.866025403784439,1.,0.866025403784439,1.))
REPRESENTATION_ITEM('')
);
#179=(
BOUNDED_CURVE()
B_SPLINE_CURVE(2,(#5402,#5403,#5404,#5405,#5406,#5407,#5408,#5409,#5410,
#5411,#5412,#5413,#5414),.UNSPECIFIED.,.F.,.F.)
B_SPLINE_CURVE_WITH_KNOTS((3,2,2,2,2,2,3),(0.462962962962963,0.469135802469136,
0.475308641975309,0.481481481481481,0.487654320987654,0.493827160493827,
0.5),.UNSPECIFIED.)
CURVE()
GEOMETRIC_REPRESENTATION_ITEM()
RATIONAL_B_SPLINE_CURVE((1.,0.866025403784439,1.,0.866025403784439,1.,0.866025403784439,
1.,0.866025403784439,1.,0.866025403784439,1.,0.866025403784439,1.))
REPRESENTATION_ITEM('')
);
#180=(
BOUNDED_CURVE()
B_SPLINE_CURVE(2,(#5415,#5416,#5417,#5418,#5419,#5420,#5421,#5422,#5423,
#5424,#5425,#5426,#5427),.UNSPECIFIED.,.F.,.F.)
B_SPLINE_CURVE_WITH_KNOTS((3,2,2,2,2,2,3),(0.462962962962963,0.469135802469136,
0.475308641975309,0.481481481481481,0.487654320987654,0.493827160493827,
0.5),.UNSPECIFIED.)
CURVE()
GEOMETRIC_REPRESENTATION_ITEM()
RATIONAL_B_SPLINE_CURVE((1.,0.866025403784439,1.,0.866025403784439,1.,0.866025403784439,
1.,0.866025403784439,1.,0.866025403784439,1.,0.866025403784439,1.))
REPRESENTATION_ITEM('')
);
#181=(
BOUNDED_CURVE()
B_SPLINE_CURVE(2,(#5432,#5433,#5434,#5435,#5436,#5437,#5438,#5439,#5440,
#5441,#5442,#5443,#5444),.UNSPECIFIED.,.F.,.F.)
B_SPLINE_CURVE_WITH_KNOTS((3,2,2,2,2,2,3),(0.425925925925926,0.432098765432099,
0.438271604938272,0.444444444444444,0.450617283950617,0.45679012345679,
0.462962962962963),.UNSPECIFIED.)
CURVE()
GEOMETRIC_REPRESENTATION_ITEM()
RATIONAL_B_SPLINE_CURVE((1.,0.866025403784439,1.,0.866025403784439,1.,0.866025403784439,
1.,0.866025403784439,1.,0.866025403784439,1.,0.866025403784439,1.))
REPRESENTATION_ITEM('')
);
#182=(
BOUNDED_CURVE()
B_SPLINE_CURVE(2,(#5445,#5446,#5447,#5448,#5449,#5450,#5451,#5452,#5453,
#5454,#5455,#5456,#5457),.UNSPECIFIED.,.F.,.F.)
B_SPLINE_CURVE_WITH_KNOTS((3,2,2,2,2,2,3),(0.425925925925926,0.432098765432099,
0.438271604938272,0.444444444444444,0.450617283950617,0.45679012345679,
0.462962962962963),.UNSPECIFIED.)
CURVE()
GEOMETRIC_REPRESENTATION_ITEM()
RATIONAL_B_SPLINE_CURVE((1.,0.866025403784439,1.,0.866025403784439,1.,0.866025403784439,
1.,0.866025403784439,1.,0.866025403784439,1.,0.866025403784439,1.))
REPRESENTATION_ITEM('')
);
#183=(
BOUNDED_CURVE()
B_SPLINE_CURVE(2,(#5462,#5463,#5464,#5465,#5466,#5467,#5468,#5469,#5470,
#5471,#5472,#5473,#5474),.UNSPECIFIED.,.F.,.F.)
B_SPLINE_CURVE_WITH_KNOTS((3,2,2,2,2,2,3),(0.388888888888889,0.395061728395062,
0.401234567901235,0.407407407407407,0.41358024691358,0.419753086419753,
0.425925925925926),.UNSPECIFIED.)
CURVE()
GEOMETRIC_REPRESENTATION_ITEM()
RATIONAL_B_SPLINE_CURVE((1.,0.866025403784439,1.,0.866025403784439,1.,0.866025403784439,
1.,0.866025403784439,1.,0.866025403784439,1.,0.866025403784439,1.))
REPRESENTATION_ITEM('')
);
#184=(
BOUNDED_CURVE()
B_SPLINE_CURVE(2,(#5475,#5476,#5477,#5478,#5479,#5480,#5481,#5482,#5483,
#5484,#5485,#5486,#5487),.UNSPECIFIED.,.F.,.F.)
B_SPLINE_CURVE_WITH_KNOTS((3,2,2,2,2,2,3),(0.388888888888889,0.395061728395062,
0.401234567901235,0.407407407407407,0.41358024691358,0.419753086419753,
0.425925925925926),.UNSPECIFIED.)
CURVE()
GEOMETRIC_REPRESENTATION_ITEM()
RATIONAL_B_SPLINE_CURVE((1.,0.866025403784439,1.,0.866025403784439,1.,0.866025403784439,
1.,0.866025403784439,1.,0.866025403784439,1.,0.866025403784439,1.))
REPRESENTATION_ITEM('')
);
#185=(
BOUNDED_CURVE()
B_SPLINE_CURVE(2,(#5492,#5493,#5494,#5495,#5496,#5497,#5498,#5499,#5500,
#5501,#5502,#5503,#5504),.UNSPECIFIED.,.F.,.F.)
B_SPLINE_CURVE_WITH_KNOTS((3,2,2,2,2,2,3),(0.351851851851852,0.358024691358025,
0.364197530864198,0.37037037037037,0.376543209876543,0.382716049382716,
0.388888888888889),.UNSPECIFIED.)
CURVE()
GEOMETRIC_REPRESENTATION_ITEM()
RATIONAL_B_SPLINE_CURVE((1.,0.866025403784439,1.,0.866025403784439,1.,0.866025403784439,
1.,0.866025403784439,1.,0.866025403784439,1.,0.866025403784439,1.))
REPRESENTATION_ITEM('')
);
#186=(
BOUNDED_CURVE()
B_SPLINE_CURVE(2,(#5505,#5506,#5507,#5508,#5509,#5510,#5511,#5512,#5513,
#5514,#5515,#5516,#5517),.UNSPECIFIED.,.F.,.F.)
B_SPLINE_CURVE_WITH_KNOTS((3,2,2,2,2,2,3),(0.351851851851852,0.358024691358025,
0.364197530864198,0.37037037037037,0.376543209876543,0.382716049382716,
0.388888888888889),.UNSPECIFIED.)
CURVE()
GEOMETRIC_REPRESENTATION_ITEM()
RATIONAL_B_SPLINE_CURVE((1.,0.866025403784439,1.,0.866025403784439,1.,0.866025403784439,
1.,0.866025403784439,1.,0.866025403784439,1.,0.866025403784439,1.))
REPRESENTATION_ITEM('')
);
#187=(
BOUNDED_CURVE()
B_SPLINE_CURVE(2,(#5522,#5523,#5524,#5525,#5526,#5527,#5528,#5529,#5530,
#5531,#5532,#5533,#5534),.UNSPECIFIED.,.F.,.F.)
B_SPLINE_CURVE_WITH_KNOTS((3,2,2,2,2,2,3),(0.314814814814815,0.320987654320988,
0.327160493827161,0.333333333333333,0.339506172839506,0.345679012345679,
0.351851851851852),.UNSPECIFIED.)
CURVE()
GEOMETRIC_REPRESENTATION_ITEM()
RATIONAL_B_SPLINE_CURVE((1.,0.866025403784439,1.,0.866025403784439,1.,0.866025403784439,
1.,0.866025403784439,1.,0.866025403784439,1.,0.866025403784439,1.))
REPRESENTATION_ITEM('')
);
#188=(
BOUNDED_CURVE()
B_SPLINE_CURVE(2,(#5535,#5536,#5537,#5538,#5539,#5540,#5541,#5542,#5543,
#5544,#5545,#5546,#5547),.UNSPECIFIED.,.F.,.F.)
B_SPLINE_CURVE_WITH_KNOTS((3,2,2,2,2,2,3),(0.314814814814815,0.320987654320988,
0.327160493827161,0.333333333333333,0.339506172839506,0.345679012345679,
0.351851851851852),.UNSPECIFIED.)
CURVE()
GEOMETRIC_REPRESENTATION_ITEM()
RATIONAL_B_SPLINE_CURVE((1.,0.866025403784439,1.,0.866025403784439,1.,0.866025403784439,
1.,0.866025403784439,1.,0.866025403784439,1.,0.866025403784439,1.))
REPRESENTATION_ITEM('')
);
#189=(
BOUNDED_CURVE()
B_SPLINE_CURVE(2,(#5552,#5553,#5554,#5555,#5556,#5557,#5558,#5559,#5560,
#5561,#5562,#5563,#5564),.UNSPECIFIED.,.F.,.F.)
B_SPLINE_CURVE_WITH_KNOTS((3,2,2,2,2,2,3),(0.277777777777778,0.283950617283951,
0.290123456790123,0.296296296296296,0.302469135802469,0.308641975308642,
0.314814814814815),.UNSPECIFIED.)
CURVE()
GEOMETRIC_REPRESENTATION_ITEM()
RATIONAL_B_SPLINE_CURVE((1.,0.866025403784439,1.,0.866025403784439,1.,0.866025403784439,
1.,0.866025403784439,1.,0.866025403784439,1.,0.866025403784439,1.))
REPRESENTATION_ITEM('')
);
#190=(
BOUNDED_CURVE()
B_SPLINE_CURVE(2,(#5565,#5566,#5567,#5568,#5569,#5570,#5571,#5572,#5573,
#5574,#5575,#5576,#5577),.UNSPECIFIED.,.F.,.F.)
B_SPLINE_CURVE_WITH_KNOTS((3,2,2,2,2,2,3),(0.277777777777778,0.283950617283951,
0.290123456790123,0.296296296296296,0.302469135802469,0.308641975308642,
0.314814814814815),.UNSPECIFIED.)
CURVE()
GEOMETRIC_REPRESENTATION_ITEM()
RATIONAL_B_SPLINE_CURVE((1.,0.866025403784439,1.,0.866025403784439,1.,0.866025403784439,
1.,0.866025403784439,1.,0.866025403784439,1.,0.866025403784439,1.))
REPRESENTATION_ITEM('')
);
#191=(
BOUNDED_CURVE()
B_SPLINE_CURVE(2,(#5582,#5583,#5584,#5585,#5586,#5587,#5588,#5589,#5590,
#5591,#5592,#5593,#5594),.UNSPECIFIED.,.F.,.F.)
B_SPLINE_CURVE_WITH_KNOTS((3,2,2,2,2,2,3),(0.240740740740741,0.246913580246914,
0.253086419753086,0.259259259259259,0.265432098765432,0.271604938271605,
0.277777777777778),.UNSPECIFIED.)
CURVE()
GEOMETRIC_REPRESENTATION_ITEM()
RATIONAL_B_SPLINE_CURVE((1.,0.866025403784439,1.,0.866025403784439,1.,0.866025403784439,
1.,0.866025403784439,1.,0.866025403784439,1.,0.866025403784439,1.))
REPRESENTATION_ITEM('')
);
#192=(
BOUNDED_CURVE()
B_SPLINE_CURVE(2,(#5595,#5596,#5597,#5598,#5599,#5600,#5601,#5602,#5603,
#5604,#5605,#5606,#5607),.UNSPECIFIED.,.F.,.F.)
B_SPLINE_CURVE_WITH_KNOTS((3,2,2,2,2,2,3),(0.240740740740741,0.246913580246914,
0.253086419753086,0.259259259259259,0.265432098765432,0.271604938271605,
0.277777777777778),.UNSPECIFIED.)
CURVE()
GEOMETRIC_REPRESENTATION_ITEM()
RATIONAL_B_SPLINE_CURVE((1.,0.866025403784439,1.,0.866025403784439,1.,0.866025403784439,
1.,0.866025403784439,1.,0.866025403784439,1.,0.866025403784439,1.))
REPRESENTATION_ITEM('')
);
#193=(
BOUNDED_CURVE()
B_SPLINE_CURVE(2,(#5612,#5613,#5614,#5615,#5616,#5617,#5618,#5619,#5620,
#5621,#5622,#5623,#5624),.UNSPECIFIED.,.F.,.F.)
B_SPLINE_CURVE_WITH_KNOTS((3,2,2,2,2,2,3),(0.203703703703704,0.209876543209877,
0.216049382716049,0.222222222222222,0.228395061728395,0.234567901234568,
0.240740740740741),.UNSPECIFIED.)
CURVE()
GEOMETRIC_REPRESENTATION_ITEM()
RATIONAL_B_SPLINE_CURVE((1.,0.866025403784439,1.,0.866025403784439,1.,0.866025403784439,
1.,0.866025403784439,1.,0.866025403784439,1.,0.866025403784439,1.))
REPRESENTATION_ITEM('')
);
#194=(
BOUNDED_CURVE()
B_SPLINE_CURVE(2,(#5625,#5626,#5627,#5628,#5629,#5630,#5631,#5632,#5633,
#5634,#5635,#5636,#5637),.UNSPECIFIED.,.F.,.F.)
B_SPLINE_CURVE_WITH_KNOTS((3,2,2,2,2,2,3),(0.203703703703704,0.209876543209877,
0.216049382716049,0.222222222222222,0.228395061728395,0.234567901234568,
0.240740740740741),.UNSPECIFIED.)
CURVE()
GEOMETRIC_REPRESENTATION_ITEM()
RATIONAL_B_SPLINE_CURVE((1.,0.866025403784439,1.,0.866025403784439,1.,0.866025403784439,
1.,0.866025403784439,1.,0.866025403784439,1.,0.866025403784439,1.))
REPRESENTATION_ITEM('')
);
#195=(
BOUNDED_CURVE()
B_SPLINE_CURVE(2,(#5642,#5643,#5644,#5645,#5646,#5647,#5648,#5649,#5650,
#5651,#5652,#5653,#5654),.UNSPECIFIED.,.F.,.F.)
B_SPLINE_CURVE_WITH_KNOTS((3,2,2,2,2,2,3),(0.166666666666667,0.172839506172839,
0.179012345679012,0.185185185185185,0.191358024691358,0.197530864197531,
0.203703703703704),.UNSPECIFIED.)
CURVE()
GEOMETRIC_REPRESENTATION_ITEM()
RATIONAL_B_SPLINE_CURVE((1.,0.866025403784439,1.,0.866025403784439,1.,0.866025403784439,
1.,0.866025403784439,1.,0.866025403784439,1.,0.866025403784439,1.))
REPRESENTATION_ITEM('')
);
#196=(
BOUNDED_CURVE()
B_SPLINE_CURVE(2,(#5655,#5656,#5657,#5658,#5659,#5660,#5661,#5662,#5663,
#5664,#5665,#5666,#5667),.UNSPECIFIED.,.F.,.F.)
B_SPLINE_CURVE_WITH_KNOTS((3,2,2,2,2,2,3),(0.166666666666667,0.172839506172839,
0.179012345679012,0.185185185185185,0.191358024691358,0.197530864197531,
0.203703703703704),.UNSPECIFIED.)
CURVE()
GEOMETRIC_REPRESENTATION_ITEM()
RATIONAL_B_SPLINE_CURVE((1.,0.866025403784439,1.,0.866025403784439,1.,0.866025403784439,
1.,0.866025403784439,1.,0.866025403784439,1.,0.866025403784439,1.))
REPRESENTATION_ITEM('')
);
#197=(
BOUNDED_CURVE()
B_SPLINE_CURVE(2,(#5672,#5673,#5674,#5675,#5676,#5677,#5678,#5679,#5680,
#5681,#5682,#5683,#5684),.UNSPECIFIED.,.F.,.F.)
B_SPLINE_CURVE_WITH_KNOTS((3,2,2,2,2,2,3),(0.12962962962963,0.135802469135802,
0.141975308641975,0.148148148148148,0.154320987654321,0.160493827160494,
0.166666666666667),.UNSPECIFIED.)
CURVE()
GEOMETRIC_REPRESENTATION_ITEM()
RATIONAL_B_SPLINE_CURVE((1.,0.866025403784439,1.,0.866025403784439,1.,0.866025403784439,
1.,0.866025403784439,1.,0.866025403784439,1.,0.866025403784439,1.))
REPRESENTATION_ITEM('')
);
#198=(
BOUNDED_CURVE()
B_SPLINE_CURVE(2,(#5685,#5686,#5687,#5688,#5689,#5690,#5691,#5692,#5693,
#5694,#5695,#5696,#5697),.UNSPECIFIED.,.F.,.F.)
B_SPLINE_CURVE_WITH_KNOTS((3,2,2,2,2,2,3),(0.12962962962963,0.135802469135802,
0.141975308641975,0.148148148148148,0.154320987654321,0.160493827160494,
0.166666666666667),.UNSPECIFIED.)
CURVE()
GEOMETRIC_REPRESENTATION_ITEM()
RATIONAL_B_SPLINE_CURVE((1.,0.866025403784439,1.,0.866025403784439,1.,0.866025403784439,
1.,0.866025403784439,1.,0.866025403784439,1.,0.866025403784439,1.))
REPRESENTATION_ITEM('')
);
#199=(
BOUNDED_CURVE()
B_SPLINE_CURVE(2,(#5702,#5703,#5704,#5705,#5706,#5707,#5708,#5709,#5710,
#5711,#5712,#5713,#5714),.UNSPECIFIED.,.F.,.F.)
B_SPLINE_CURVE_WITH_KNOTS((3,2,2,2,2,2,3),(0.0925925925925926,0.0987654320987654,
0.104938271604938,0.111111111111111,0.117283950617284,0.123456790123457,
0.12962962962963),.UNSPECIFIED.)
CURVE()
GEOMETRIC_REPRESENTATION_ITEM()
RATIONAL_B_SPLINE_CURVE((1.,0.866025403784439,1.,0.866025403784439,1.,0.866025403784439,
1.,0.866025403784439,1.,0.866025403784439,1.,0.866025403784439,1.))
REPRESENTATION_ITEM('')
);
#200=(
BOUNDED_CURVE()
B_SPLINE_CURVE(2,(#5715,#5716,#5717,#5718,#5719,#5720,#5721,#5722,#5723,
#5724,#5725,#5726,#5727),.UNSPECIFIED.,.F.,.F.)
B_SPLINE_CURVE_WITH_KNOTS((3,2,2,2,2,2,3),(0.0925925925925926,0.0987654320987654,
0.104938271604938,0.111111111111111,0.117283950617284,0.123456790123457,
0.12962962962963),.UNSPECIFIED.)
CURVE()
GEOMETRIC_REPRESENTATION_ITEM()
RATIONAL_B_SPLINE_CURVE((1.,0.866025403784439,1.,0.866025403784439,1.,0.866025403784439,
1.,0.866025403784439,1.,0.866025403784439,1.,0.866025403784439,1.))
REPRESENTATION_ITEM('')
);
#201=(
BOUNDED_CURVE()
B_SPLINE_CURVE(2,(#5732,#5733,#5734,#5735,#5736,#5737,#5738,#5739,#5740,
#5741,#5742,#5743,#5744),.UNSPECIFIED.,.F.,.F.)
B_SPLINE_CURVE_WITH_KNOTS((3,2,2,2,2,2,3),(0.0555555555555556,0.0617283950617284,
0.0679012345679012,0.0740740740740741,0.0802469135802469,0.0864197530864197,
0.0925925925925926),.UNSPECIFIED.)
CURVE()
GEOMETRIC_REPRESENTATION_ITEM()
RATIONAL_B_SPLINE_CURVE((1.,0.866025403784439,1.,0.866025403784439,1.,0.866025403784439,
1.,0.866025403784439,1.,0.866025403784439,1.,0.866025403784439,1.))
REPRESENTATION_ITEM('')
);
#202=(
BOUNDED_CURVE()
B_SPLINE_CURVE(2,(#5745,#5746,#5747,#5748,#5749,#5750,#5751,#5752,#5753,
#5754,#5755,#5756,#5757),.UNSPECIFIED.,.F.,.F.)
B_SPLINE_CURVE_WITH_KNOTS((3,2,2,2,2,2,3),(0.0555555555555556,0.0617283950617284,
0.0679012345679012,0.0740740740740741,0.0802469135802469,0.0864197530864197,
0.0925925925925926),.UNSPECIFIED.)
CURVE()
GEOMETRIC_REPRESENTATION_ITEM()
RATIONAL_B_SPLINE_CURVE((1.,0.866025403784439,1.,0.866025403784439,1.,0.866025403784439,
1.,0.866025403784439,1.,0.866025403784439,1.,0.866025403784439,1.))
REPRESENTATION_ITEM('')
);
#203=(
BOUNDED_CURVE()
B_SPLINE_CURVE(2,(#5762,#5763,#5764,#5765,#5766,#5767,#5768,#5769,#5770,
#5771,#5772,#5773,#5774),.UNSPECIFIED.,.F.,.F.)
B_SPLINE_CURVE_WITH_KNOTS((3,2,2,2,2,2,3),(0.0185185185185185,0.0246913580246914,
0.0308641975308642,0.037037037037037,0.0432098765432099,0.0493827160493827,
0.0555555555555556),.UNSPECIFIED.)
CURVE()
GEOMETRIC_REPRESENTATION_ITEM()
RATIONAL_B_SPLINE_CURVE((1.,0.866025403784439,1.,0.866025403784439,1.,0.866025403784439,
1.,0.866025403784439,1.,0.866025403784439,1.,0.866025403784439,1.))
REPRESENTATION_ITEM('')
);
#204=(
BOUNDED_CURVE()
B_SPLINE_CURVE(2,(#5775,#5776,#5777,#5778,#5779,#5780,#5781,#5782,#5783,
#5784,#5785,#5786,#5787),.UNSPECIFIED.,.F.,.F.)
B_SPLINE_CURVE_WITH_KNOTS((3,2,2,2,2,2,3),(0.0185185185185185,0.0246913580246914,
0.0308641975308642,0.037037037037037,0.0432098765432099,0.0493827160493827,
0.0555555555555556),.UNSPECIFIED.)
CURVE()
GEOMETRIC_REPRESENTATION_ITEM()
RATIONAL_B_SPLINE_CURVE((1.,0.866025403784439,1.,0.866025403784439,1.,0.866025403784439,
1.,0.866025403784439,1.,0.866025403784439,1.,0.866025403784439,1.))
REPRESENTATION_ITEM('')
);
#205=(
BOUNDED_CURVE()
B_SPLINE_CURVE(2,(#8530,#8531,#8532,#8533,#8534,#8535,#8536),
 .UNSPECIFIED.,.F.,.F.)
B_SPLINE_CURVE_WITH_KNOTS((3,2,2,3),(0.,0.00617283950617284,0.0123456790123457,
0.0185185185185185),.UNSPECIFIED.)
CURVE()
GEOMETRIC_REPRESENTATION_ITEM()
RATIONAL_B_SPLINE_CURVE((1.,0.866025403784439,1.,0.866025403784439,1.,0.866025403784439,
1.))
REPRESENTATION_ITEM('')
);
#206=(
BOUNDED_CURVE()
B_SPLINE_CURVE(2,(#8538,#8539,#8540,#8541,#8542,#8543,#8544),
 .UNSPECIFIED.,.F.,.F.)
B_SPLINE_CURVE_WITH_KNOTS((3,2,2,3),(0.,0.00617283950617284,0.0123456790123457,
0.0185185185185185),.UNSPECIFIED.)
CURVE()
GEOMETRIC_REPRESENTATION_ITEM()
RATIONAL_B_SPLINE_CURVE((1.,0.866025403784439,1.,0.866025403784439,1.,0.866025403784439,
1.))
REPRESENTATION_ITEM('')
);
#207=(
BOUNDED_CURVE()
B_SPLINE_CURVE(2,(#11079,#11080,#11081,#11082,#11083,#11084,#11085,#11086,
#11087,#11088,#11089,#11090,#11091,#11092,#11093,#11094,#11095,#11096,#11097,
#11098,#11099,#11100,#11101,#11102,#11103,#11104,#11105,#11106,#11107,#11108,
#11109,#11110,#11111,#11112,#11113,#11114,#11115,#11116,#11117,#11118,#11119,
#11120,#11121,#11122,#11123,#11124,#11125,#11126,#11127,#11128,#11129,#11130,
#11131,#11132,#11133,#11134,#11135,#11136,#11137,#11138,#11139,#11140,#11141,
#11142,#11143,#11144,#11145,#11146,#11147,#11148,#11149,#11150,#11151,#11152,
#11153,#11154,#11155,#11156,#11157,#11158,#11159,#11160,#11161,#11162,#11163,
#11164,#11165,#11166,#11167,#11168,#11169,#11170,#11171,#11172,#11173,#11174,
#11175,#11176,#11177,#11178,#11179,#11180,#11181,#11182,#11183,#11184,#11185,
#11186,#11187,#11188,#11189,#11190,#11191,#11192,#11193,#11194,#11195,#11196,
#11197,#11198,#11199,#11200,#11201,#11202,#11203,#11204,#11205,#11206,#11207,
#11208,#11209,#11210,#11211,#11212,#11213,#11214,#11215,#11216,#11217,#11218,
#11219,#11220,#11221,#11222,#11223,#11224,#11225,#11226,#11227,#11228,#11229,
#11230,#11231,#11232,#11233,#11234,#11235,#11236,#11237,#11238,#11239,#11240,
#11241,#11242,#11243,#11244,#11245,#11246,#11247,#11248,#11249,#11250,#11251,
#11252,#11253,#11254,#11255,#11256,#11257,#11258,#11259,#11260,#11261,#11262,
#11263,#11264,#11265,#11266,#11267,#11268,#11269,#11270,#11271,#11272,#11273,
#11274,#11275,#11276,#11277,#11278,#11279,#11280,#11281,#11282,#11283,#11284,
#11285,#11286,#11287,#11288,#11289,#11290,#11291,#11292,#11293,#11294,#11295,
#11296,#11297,#11298,#11299,#11300,#11301,#11302,#11303,#11304,#11305,#11306,
#11307,#11308,#11309,#11310,#11311,#11312,#11313,#11314,#11315,#11316,#11317),
 .UNSPECIFIED.,.F.,.F.)
B_SPLINE_CURVE_WITH_KNOTS((3,2,2,2,2,2,2,2,2,2,2,2,2,2,2,2,2,2,2,2,2,2,
2,2,2,2,2,2,2,2,2,2,2,2,2,2,2,2,2,2,2,2,2,2,2,2,2,2,2,2,2,2,2,2,2,2,2,2,
2,2,2,2,2,2,2,2,2,2,2,2,2,2,2,2,2,2,2,2,2,2,2,2,2,2,2,2,2,2,2,2,2,2,2,2,
2,2,2,2,2,2,2,2,2,2,2,2,2,2,2,2,2,2,2,2,2,2,2,2,2,3),(0.0150916102575603,
0.0166666666666667,0.025,0.0333333333333333,0.0416666666666667,0.05,0.0583333333333333,
0.0666666666666667,0.075,0.0833333333333333,0.0916666666666667,0.1,0.108333333333333,
0.116666666666667,0.125,0.133333333333333,0.141666666666667,0.15,0.158333333333333,
0.166666666666667,0.175,0.183333333333333,0.191666666666667,0.2,0.208333333333333,
0.216666666666667,0.225,0.233333333333333,0.241666666666667,0.25,0.258333333333333,
0.266666666666667,0.275,0.283333333333333,0.291666666666667,0.3,0.308333333333333,
0.316666666666667,0.325,0.333333333333333,0.341666666666667,0.35,0.358333333333333,
0.366666666666667,0.375,0.383333333333333,0.391666666666667,0.4,0.408333333333333,
0.416666666666667,0.425,0.433333333333333,0.441666666666667,0.45,0.458333333333333,
0.466666666666667,0.475,0.483333333333333,0.491666666666667,0.5,0.508333333333333,
0.516666666666667,0.525,0.533333333333333,0.541666666666667,0.55,0.558333333333333,
0.566666666666667,0.575,0.583333333333333,0.591666666666667,0.6,0.608333333333333,
0.616666666666667,0.625,0.633333333333333,0.641666666666667,0.65,0.658333333333333,
0.666666666666667,0.675,0.683333333333333,0.691666666666667,0.7,0.708333333333333,
0.716666666666667,0.725,0.733333333333333,0.741666666666667,0.75,0.758333333333333,
0.766666666666667,0.775,0.783333333333333,0.791666666666667,0.8,0.808333333333333,
0.816666666666667,0.825,0.833333333333333,0.841666666666667,0.85,0.858333333333333,
0.866666666666667,0.875,0.883333333333333,0.891666666666667,0.9,0.908333333333333,
0.916666666666667,0.925,0.933333333333333,0.941666666666667,0.95,0.958333333333333,
0.966666666666667,0.975,0.983333333333333,0.991666666666667,1.),
 .UNSPECIFIED.)
CURVE()
GEOMETRIC_REPRESENTATION_ITEM()
RATIONAL_B_SPLINE_CURVE((0.989554002528501,0.993559750517391,1.,0.965925826289068,
1.,0.965925826289068,1.,0.965925826289068,1.,0.965925826289068,1.,0.965925826289068,
1.,0.965925826289068,1.,0.965925826289068,1.,0.965925826289068,1.,0.965925826289068,
1.,0.965925826289068,1.,0.965925826289068,1.,0.965925826289068,1.,0.965925826289068,
1.,0.965925826289068,1.,0.965925826289068,1.,0.965925826289068,1.,0.965925826289068,
1.,0.965925826289068,1.,0.965925826289068,1.,0.965925826289068,1.,0.965925826289068,
1.,0.965925826289068,1.,0.965925826289068,1.,0.965925826289068,1.,0.965925826289068,
1.,0.965925826289068,1.,0.965925826289068,1.,0.965925826289068,1.,0.965925826289068,
1.,0.965925826289068,1.,0.965925826289068,1.,0.965925826289068,1.,0.965925826289068,
1.,0.965925826289068,1.,0.965925826289068,1.,0.965925826289068,1.,0.965925826289068,
1.,0.965925826289068,1.,0.965925826289068,1.,0.965925826289068,1.,0.965925826289068,
1.,0.965925826289068,1.,0.965925826289068,1.,0.965925826289068,1.,0.965925826289068,
1.,0.965925826289068,1.,0.965925826289068,1.,0.965925826289068,1.,0.965925826289068,
1.,0.965925826289068,1.,0.965925826289068,1.,0.965925826289068,1.,0.965925826289068,
1.,0.965925826289068,1.,0.965925826289068,1.,0.965925826289068,1.,0.965925826289068,
1.,0.965925826289068,1.,0.965925826289068,1.,0.965925826289068,1.,0.965925826289068,
1.,0.965925826289068,1.,0.965925826289068,1.,0.965925826289068,1.,0.965925826289068,
1.,0.965925826289068,1.,0.965925826289068,1.,0.965925826289068,1.,0.965925826289068,
1.,0.965925826289068,1.,0.965925826289068,1.,0.965925826289068,1.,0.965925826289068,
1.,0.965925826289068,1.,0.965925826289068,1.,0.965925826289068,1.,0.965925826289068,
1.,0.965925826289068,1.,0.965925826289068,1.,0.965925826289068,1.,0.965925826289068,
1.,0.965925826289068,1.,0.965925826289068,1.,0.965925826289068,1.,0.965925826289068,
1.,0.965925826289068,1.,0.965925826289068,1.,0.965925826289068,1.,0.965925826289068,
1.,0.965925826289068,1.,0.965925826289068,1.,0.965925826289068,1.,0.965925826289068,
1.,0.965925826289068,1.,0.965925826289068,1.,0.965925826289068,1.,0.965925826289068,
1.,0.965925826289068,1.,0.965925826289068,1.,0.965925826289068,1.,0.965925826289068,
1.,0.965925826289068,1.,0.965925826289068,1.,0.965925826289068,1.,0.965925826289068,
1.,0.965925826289068,1.,0.965925826289068,1.,0.965925826289068,1.,0.965925826289068,
1.,0.965925826289068,1.,0.965925826289068,1.,0.965925826289068,1.,0.965925826289068,
1.,0.965925826289068,1.,0.965925826289068,1.,0.965925826289068,1.,0.965925826289068,
1.,0.965925826289068,1.))
REPRESENTATION_ITEM('')
);
#208=(
BOUNDED_CURVE()
B_SPLINE_CURVE(2,(#11321,#11322,#11323,#11324,#11325,#11326,#11327,#11328,
#11329,#11330,#11331,#11332,#11333,#11334,#11335,#11336,#11337,#11338,#11339,
#11340,#11341,#11342,#11343,#11344,#11345,#11346,#11347,#11348,#11349,#11350,
#11351,#11352,#11353,#11354,#11355,#11356,#11357,#11358,#11359,#11360,#11361,
#11362,#11363,#11364,#11365,#11366,#11367,#11368,#11369,#11370,#11371,#11372,
#11373,#11374,#11375,#11376,#11377,#11378,#11379,#11380,#11381,#11382,#11383,
#11384,#11385,#11386,#11387,#11388,#11389,#11390,#11391,#11392,#11393,#11394,
#11395,#11396,#11397,#11398,#11399,#11400,#11401,#11402,#11403,#11404,#11405,
#11406,#11407,#11408,#11409,#11410,#11411,#11412,#11413,#11414,#11415,#11416,
#11417,#11418,#11419,#11420,#11421,#11422,#11423,#11424,#11425,#11426,#11427,
#11428,#11429,#11430,#11431,#11432,#11433,#11434,#11435,#11436,#11437,#11438,
#11439,#11440,#11441,#11442,#11443,#11444,#11445,#11446,#11447,#11448,#11449,
#11450,#11451,#11452,#11453,#11454,#11455,#11456,#11457,#11458,#11459,#11460,
#11461,#11462,#11463,#11464,#11465,#11466,#11467,#11468,#11469,#11470,#11471,
#11472,#11473,#11474,#11475,#11476,#11477,#11478,#11479,#11480,#11481,#11482,
#11483,#11484,#11485,#11486,#11487,#11488,#11489,#11490,#11491,#11492,#11493,
#11494,#11495,#11496,#11497,#11498,#11499,#11500,#11501,#11502,#11503,#11504,
#11505,#11506,#11507,#11508,#11509,#11510,#11511,#11512,#11513,#11514,#11515,
#11516,#11517,#11518,#11519,#11520,#11521,#11522,#11523,#11524,#11525,#11526,
#11527,#11528,#11529,#11530,#11531,#11532,#11533,#11534,#11535,#11536,#11537,
#11538,#11539,#11540,#11541,#11542,#11543,#11544,#11545,#11546,#11547,#11548,
#11549,#11550,#11551,#11552,#11553,#11554,#11555,#11556,#11557,#11558,#11559,
#11560,#11561),.UNSPECIFIED.,.F.,.F.)
B_SPLINE_CURVE_WITH_KNOTS((3,2,2,2,2,2,2,2,2,2,2,2,2,2,2,2,2,2,2,2,2,2,
2,2,2,2,2,2,2,2,2,2,2,2,2,2,2,2,2,2,2,2,2,2,2,2,2,2,2,2,2,2,2,2,2,2,2,2,
2,2,2,2,2,2,2,2,2,2,2,2,2,2,2,2,2,2,2,2,2,2,2,2,2,2,2,2,2,2,2,2,2,2,2,2,
2,2,2,2,2,2,2,2,2,2,2,2,2,2,2,2,2,2,2,2,2,2,2,2,2,2,3),(0.,0.00833333333333333,
0.0166666666666667,0.025,0.0333333333333333,0.0416666666666667,0.05,0.0583333333333333,
0.0666666666666667,0.075,0.0833333333333333,0.0916666666666667,0.1,0.108333333333333,
0.116666666666667,0.125,0.133333333333333,0.141666666666667,0.15,0.158333333333333,
0.166666666666667,0.175,0.183333333333333,0.191666666666667,0.2,0.208333333333333,
0.216666666666667,0.225,0.233333333333333,0.241666666666667,0.25,0.258333333333333,
0.266666666666667,0.275,0.283333333333333,0.291666666666667,0.3,0.308333333333333,
0.316666666666667,0.325,0.333333333333333,0.341666666666667,0.35,0.358333333333333,
0.366666666666667,0.375,0.383333333333333,0.391666666666667,0.4,0.408333333333333,
0.416666666666667,0.425,0.433333333333333,0.441666666666667,0.45,0.458333333333333,
0.466666666666667,0.475,0.483333333333333,0.491666666666667,0.5,0.508333333333333,
0.516666666666667,0.525,0.533333333333333,0.541666666666667,0.55,0.558333333333333,
0.566666666666667,0.575,0.583333333333333,0.591666666666667,0.6,0.608333333333333,
0.616666666666667,0.625,0.633333333333333,0.641666666666667,0.65,0.658333333333333,
0.666666666666667,0.675,0.683333333333333,0.691666666666667,0.7,0.708333333333333,
0.716666666666667,0.725,0.733333333333333,0.741666666666667,0.75,0.758333333333333,
0.766666666666667,0.775,0.783333333333333,0.791666666666667,0.8,0.808333333333333,
0.816666666666667,0.825,0.833333333333333,0.841666666666667,0.85,0.858333333333333,
0.866666666666667,0.875,0.883333333333333,0.891666666666667,0.9,0.908333333333333,
0.916666666666667,0.925,0.933333333333333,0.941666666666667,0.95,0.958333333333333,
0.966666666666667,0.975,0.983333333333333,0.991666666666667,1.),
 .UNSPECIFIED.)
CURVE()
GEOMETRIC_REPRESENTATION_ITEM()
RATIONAL_B_SPLINE_CURVE((1.,0.965925826289068,1.,0.965925826289068,1.,0.965925826289068,
1.,0.965925826289068,1.,0.965925826289068,1.,0.965925826289068,1.,0.965925826289068,
1.,0.965925826289068,1.,0.965925826289068,1.,0.965925826289068,1.,0.965925826289068,
1.,0.965925826289068,1.,0.965925826289068,1.,0.965925826289068,1.,0.965925826289068,
1.,0.965925826289068,1.,0.965925826289068,1.,0.965925826289068,1.,0.965925826289068,
1.,0.965925826289068,1.,0.965925826289068,1.,0.965925826289068,1.,0.965925826289068,
1.,0.965925826289068,1.,0.965925826289068,1.,0.965925826289068,1.,0.965925826289068,
1.,0.965925826289068,1.,0.965925826289068,1.,0.965925826289068,1.,0.965925826289068,
1.,0.965925826289068,1.,0.965925826289068,1.,0.965925826289068,1.,0.965925826289068,
1.,0.965925826289068,1.,0.965925826289068,1.,0.965925826289068,1.,0.965925826289068,
1.,0.965925826289068,1.,0.965925826289068,1.,0.965925826289068,1.,0.965925826289068,
1.,0.965925826289068,1.,0.965925826289068,1.,0.965925826289068,1.,0.965925826289068,
1.,0.965925826289068,1.,0.965925826289068,1.,0.965925826289068,1.,0.965925826289068,
1.,0.965925826289068,1.,0.965925826289068,1.,0.965925826289068,1.,0.965925826289068,
1.,0.965925826289068,1.,0.965925826289068,1.,0.965925826289068,1.,0.965925826289068,
1.,0.965925826289068,1.,0.965925826289068,1.,0.965925826289068,1.,0.965925826289068,
1.,0.965925826289068,1.,0.965925826289068,1.,0.965925826289068,1.,0.965925826289068,
1.,0.965925826289068,1.,0.965925826289068,1.,0.965925826289068,1.,0.965925826289068,
1.,0.965925826289068,1.,0.965925826289068,1.,0.965925826289068,1.,0.965925826289068,
1.,0.965925826289068,1.,0.965925826289068,1.,0.965925826289068,1.,0.965925826289068,
1.,0.965925826289068,1.,0.965925826289068,1.,0.965925826289068,1.,0.965925826289068,
1.,0.965925826289068,1.,0.965925826289068,1.,0.965925826289068,1.,0.965925826289068,
1.,0.965925826289068,1.,0.965925826289068,1.,0.965925826289068,1.,0.965925826289068,
1.,0.965925826289068,1.,0.965925826289068,1.,0.965925826289068,1.,0.965925826289068,
1.,0.965925826289068,1.,0.965925826289068,1.,0.965925826289068,1.,0.965925826289068,
1.,0.965925826289068,1.,0.965925826289068,1.,0.965925826289068,1.,0.965925826289068,
1.,0.965925826289068,1.,0.965925826289068,1.,0.965925826289068,1.,0.965925826289068,
1.,0.965925826289068,1.,0.965925826289068,1.,0.965925826289068,1.,0.965925826289068,
1.,0.965925826289068,1.,0.965925826289068,1.,0.965925826289068,1.,0.965925826289068,
1.,0.965925826289068,1.,0.965925826289068,1.,0.965925826289068,1.,0.965925826289068,
1.,0.965925826289068,1.))
REPRESENTATION_ITEM('')
);
#209=(
BOUNDED_CURVE()
B_SPLINE_CURVE(2,(#13443,#13444,#13445),.UNSPECIFIED.,.F.,.F.)
B_SPLINE_CURVE_WITH_KNOTS((3,3),(1.19691741652703,2.09556504436786),
 .UNSPECIFIED.)
CURVE()
GEOMETRIC_REPRESENTATION_ITEM()
RATIONAL_B_SPLINE_CURVE((1.52268468506016,1.64046475534049,1.64046475534049))
REPRESENTATION_ITEM('')
);
#210=(
BOUNDED_CURVE()
B_SPLINE_CURVE(2,(#13446,#13447,#13448),.UNSPECIFIED.,.F.,.F.)
B_SPLINE_CURVE_WITH_KNOTS((3,3),(2.09556504436786,2.9942126722087),
 .UNSPECIFIED.)
CURVE()
GEOMETRIC_REPRESENTATION_ITEM()
RATIONAL_B_SPLINE_CURVE((1.64046475534049,1.64046475534049,1.52268468506016))
REPRESENTATION_ITEM('')
);
#211=(
BOUNDED_CURVE()
B_SPLINE_CURVE(2,(#13491,#13492,#13493),.UNSPECIFIED.,.F.,.F.)
B_SPLINE_CURVE_WITH_KNOTS((3,3),(1.19691741652693,2.09556504436774),
 .UNSPECIFIED.)
CURVE()
GEOMETRIC_REPRESENTATION_ITEM()
RATIONAL_B_SPLINE_CURVE((1.52268468506012,1.64046475534044,1.64046475534044))
REPRESENTATION_ITEM('')
);
#212=(
BOUNDED_CURVE()
B_SPLINE_CURVE(2,(#13494,#13495,#13496),.UNSPECIFIED.,.F.,.F.)
B_SPLINE_CURVE_WITH_KNOTS((3,3),(2.09556504436774,2.99421267220854),
 .UNSPECIFIED.)
CURVE()
GEOMETRIC_REPRESENTATION_ITEM()
RATIONAL_B_SPLINE_CURVE((1.64046475534044,1.64046475534044,1.52268468506012))
REPRESENTATION_ITEM('')
);
#213=(
BOUNDED_CURVE()
B_SPLINE_CURVE(2,(#13539,#13540,#13541),.UNSPECIFIED.,.F.,.F.)
B_SPLINE_CURVE_WITH_KNOTS((3,3),(2.09556504652211,2.99421267491808),
 .UNSPECIFIED.)
CURVE()
GEOMETRIC_REPRESENTATION_ITEM()
RATIONAL_B_SPLINE_CURVE((1.64046475620257,1.64046475620257,1.52268468586035))
REPRESENTATION_ITEM('')
);
#214=(
BOUNDED_CURVE()
B_SPLINE_CURVE(2,(#13542,#13543,#13544),.UNSPECIFIED.,.F.,.F.)
B_SPLINE_CURVE_WITH_KNOTS((3,3),(1.19691741812614,2.09556504652211),
 .UNSPECIFIED.)
CURVE()
GEOMETRIC_REPRESENTATION_ITEM()
RATIONAL_B_SPLINE_CURVE((1.52268468586035,1.64046475620257,1.64046475620257))
REPRESENTATION_ITEM('')
);
#215=(
BOUNDED_CURVE()
B_SPLINE_CURVE(2,(#13587,#13588,#13589),.UNSPECIFIED.,.F.,.F.)
B_SPLINE_CURVE_WITH_KNOTS((3,3),(1.19691741652704,2.09556504436788),
 .UNSPECIFIED.)
CURVE()
GEOMETRIC_REPRESENTATION_ITEM()
RATIONAL_B_SPLINE_CURVE((1.52268468506017,1.6404647553405,1.6404647553405))
REPRESENTATION_ITEM('')
);
#216=(
BOUNDED_CURVE()
B_SPLINE_CURVE(2,(#13590,#13591,#13592),.UNSPECIFIED.,.F.,.F.)
B_SPLINE_CURVE_WITH_KNOTS((3,3),(2.09556504436788,2.99421267220872),
 .UNSPECIFIED.)
CURVE()
GEOMETRIC_REPRESENTATION_ITEM()
RATIONAL_B_SPLINE_CURVE((1.6404647553405,1.6404647553405,1.52268468506017))
REPRESENTATION_ITEM('')
);
#217=(
BOUNDED_CURVE()
B_SPLINE_CURVE(2,(#13635,#13636,#13637),.UNSPECIFIED.,.F.,.F.)
B_SPLINE_CURVE_WITH_KNOTS((3,3),(1.19691741652693,2.09556504436774),
 .UNSPECIFIED.)
CURVE()
GEOMETRIC_REPRESENTATION_ITEM()
RATIONAL_B_SPLINE_CURVE((1.52268468506012,1.64046475534044,1.64046475534044))
REPRESENTATION_ITEM('')
);
#218=(
BOUNDED_CURVE()
B_SPLINE_CURVE(2,(#13638,#13639,#13640),.UNSPECIFIED.,.F.,.F.)
B_SPLINE_CURVE_WITH_KNOTS((3,3),(2.09556504436774,2.99421267220854),
 .UNSPECIFIED.)
CURVE()
GEOMETRIC_REPRESENTATION_ITEM()
RATIONAL_B_SPLINE_CURVE((1.64046475534044,1.64046475534044,1.52268468506012))
REPRESENTATION_ITEM('')
);
#219=(
BOUNDED_CURVE()
B_SPLINE_CURVE(2,(#13680,#13681,#13682),.UNSPECIFIED.,.F.,.F.)
B_SPLINE_CURVE_WITH_KNOTS((3,3),(1.19691742009084,2.09556504916886),
 .UNSPECIFIED.)
CURVE()
GEOMETRIC_REPRESENTATION_ITEM()
RATIONAL_B_SPLINE_CURVE((1.52268468684348,1.64046475726175,1.64046475726175))
REPRESENTATION_ITEM('')
);
#220=(
BOUNDED_CURVE()
B_SPLINE_CURVE(2,(#13683,#13684,#13685),.UNSPECIFIED.,.F.,.F.)
B_SPLINE_CURVE_WITH_KNOTS((3,3),(2.09556504916886,2.99421267824688),
 .UNSPECIFIED.)
CURVE()
GEOMETRIC_REPRESENTATION_ITEM()
RATIONAL_B_SPLINE_CURVE((1.64046475726175,1.64046475726175,1.52268468684348))
REPRESENTATION_ITEM('')
);
#221=SHAPE_REPRESENTATION_RELATIONSHIP('SRR','None',#14120,#230);
#222=SHAPE_REPRESENTATION_RELATIONSHIP('SRR','None',#14121,#231);
#223=SHAPE_REPRESENTATION_RELATIONSHIP('SRR','None',#14122,#232);
#224=SHAPE_REPRESENTATION_RELATIONSHIP('SRR','None',#14123,#233);
#225=SHAPE_REPRESENTATION_RELATIONSHIP('SRR','None',#14124,#234);
#226=SHAPE_REPRESENTATION_RELATIONSHIP('SRR','None',#14125,#235);
#227=SHAPE_REPRESENTATION_RELATIONSHIP('SRR','None',#14126,#236);
#228=SHAPE_REPRESENTATION_RELATIONSHIP('SRR','None',#14127,#237);
#229=SHAPE_REPRESENTATION_RELATIONSHIP('SRR','None',#14128,#238);
#230=ADVANCED_BREP_SHAPE_REPRESENTATION('',(#248),#14075);
#231=ADVANCED_BREP_SHAPE_REPRESENTATION('',(#249),#14076);
#232=ADVANCED_BREP_SHAPE_REPRESENTATION('',(#250),#14077);
#233=ADVANCED_BREP_SHAPE_REPRESENTATION('',(#251),#14078);
#234=ADVANCED_BREP_SHAPE_REPRESENTATION('',(#252),#14079);
#235=ADVANCED_BREP_SHAPE_REPRESENTATION('',(#253),#14080);
#236=ADVANCED_BREP_SHAPE_REPRESENTATION('',(#254),#14081);
#237=ADVANCED_BREP_SHAPE_REPRESENTATION('',(#255),#14082);
#238=ADVANCED_BREP_SHAPE_REPRESENTATION('',(#256),#14083);
#239=STYLED_ITEM('',(#14174),#248);
#240=STYLED_ITEM('',(#14175),#249);
#241=STYLED_ITEM('',(#14176),#250);
#242=STYLED_ITEM('',(#14175),#251);
#243=STYLED_ITEM('',(#14175),#252);
#244=STYLED_ITEM('',(#14175),#253);
#245=STYLED_ITEM('',(#14176),#254);
#246=STYLED_ITEM('',(#14177),#255);
#247=STYLED_ITEM('',(#14178),#256);
#248=MANIFOLD_SOLID_BREP('Body1',#3465);
#249=MANIFOLD_SOLID_BREP('Body1',#3466);
#250=MANIFOLD_SOLID_BREP('Body1',#3467);
#251=MANIFOLD_SOLID_BREP('Body1',#3468);
#252=MANIFOLD_SOLID_BREP('Body1',#3469);
#253=MANIFOLD_SOLID_BREP('Body1',#3470);
#254=MANIFOLD_SOLID_BREP('Body1',#3471);
#255=MANIFOLD_SOLID_BREP('Body1',#3472);
#256=MANIFOLD_SOLID_BREP('Body1',#3473);
#257=FACE_BOUND('',#558,.T.);
#258=FACE_BOUND('',#561,.T.);
#259=FACE_BOUND('',#580,.T.);
#260=FACE_BOUND('',#590,.T.);
#261=FACE_BOUND('',#593,.T.);
#262=FACE_BOUND('',#599,.T.);
#263=FACE_BOUND('',#601,.T.);
#264=FACE_BOUND('',#603,.T.);
#265=FACE_BOUND('',#673,.T.);
#266=FACE_BOUND('',#675,.T.);
#267=FACE_BOUND('',#687,.T.);
#268=FACE_BOUND('',#689,.T.);
#269=FACE_BOUND('',#691,.T.);
#270=FACE_BOUND('',#697,.T.);
#271=FACE_BOUND('',#699,.T.);
#272=FACE_BOUND('',#701,.T.);
#273=FACE_BOUND('',#716,.T.);
#274=FACE_BOUND('',#717,.T.);
#275=FACE_BOUND('',#719,.T.);
#276=FACE_BOUND('',#720,.T.);
#277=FACE_BOUND('',#725,.T.);
#278=FACE_BOUND('',#726,.T.);
#279=FACE_BOUND('',#728,.T.);
#280=FACE_BOUND('',#729,.T.);
#281=FACE_BOUND('',#749,.T.);
#282=FACE_BOUND('',#751,.T.);
#283=FACE_BOUND('',#769,.T.);
#284=FACE_BOUND('',#772,.T.);
#285=PLANE('',#3582);
#286=PLANE('',#3586);
#287=PLANE('',#3587);
#288=PLANE('',#3588);
#289=PLANE('',#3589);
#290=PLANE('',#3590);
#291=PLANE('',#3591);
#292=PLANE('',#3592);
#293=PLANE('',#3593);
#294=PLANE('',#3594);
#295=PLANE('',#3595);
#296=PLANE('',#3596);
#297=PLANE('',#3613);
#298=PLANE('',#3614);
#299=PLANE('',#3615);
#300=PLANE('',#3617);
#301=PLANE('',#3618);
#302=PLANE('',#3619);
#303=PLANE('',#3620);
#304=PLANE('',#3621);
#305=PLANE('',#3622);
#306=PLANE('',#3623);
#307=PLANE('',#3624);
#308=PLANE('',#3625);
#309=PLANE('',#3627);
#310=PLANE('',#3628);
#311=PLANE('',#3631);
#312=PLANE('',#3632);
#313=PLANE('',#3633);
#314=PLANE('',#3634);
#315=PLANE('',#3636);
#316=PLANE('',#3638);
#317=PLANE('',#3640);
#318=PLANE('',#3641);
#319=PLANE('',#3642);
#320=PLANE('',#3643);
#321=PLANE('',#3645);
#322=PLANE('',#3646);
#323=PLANE('',#3647);
#324=PLANE('',#3718);
#325=PLANE('',#3719);
#326=PLANE('',#3720);
#327=PLANE('',#3721);
#328=PLANE('',#3722);
#329=PLANE('',#3723);
#330=PLANE('',#3738);
#331=PLANE('',#3739);
#332=PLANE('',#3740);
#333=PLANE('',#3752);
#334=PLANE('',#3753);
#335=PLANE('',#3754);
#336=PLANE('',#3757);
#337=PLANE('',#3760);
#338=PLANE('',#3779);
#339=PLANE('',#3780);
#340=PLANE('',#3781);
#341=PLANE('',#3782);
#342=PLANE('',#3783);
#343=PLANE('',#3784);
#344=PLANE('',#3785);
#345=PLANE('',#3786);
#346=PLANE('',#3787);
#347=PLANE('',#3788);
#348=PLANE('',#3789);
#349=PLANE('',#3791);
#350=PLANE('',#3797);
#351=PLANE('',#3800);
#352=PLANE('',#3801);
#353=PLANE('',#3820);
#354=PLANE('',#3821);
#355=PLANE('',#3822);
#356=PLANE('',#3823);
#357=PLANE('',#3824);
#358=PLANE('',#3825);
#359=PLANE('',#3826);
#360=PLANE('',#3833);
#361=PLANE('',#3850);
#362=PLANE('',#3851);
#363=PLANE('',#3852);
#364=PLANE('',#3853);
#365=FACE_OUTER_BOUND('',#555,.T.);
#366=FACE_OUTER_BOUND('',#556,.T.);
#367=FACE_OUTER_BOUND('',#557,.T.);
#368=FACE_OUTER_BOUND('',#559,.T.);
#369=FACE_OUTER_BOUND('',#560,.T.);
#370=FACE_OUTER_BOUND('',#562,.T.);
#371=FACE_OUTER_BOUND('',#563,.T.);
#372=FACE_OUTER_BOUND('',#564,.T.);
#373=FACE_OUTER_BOUND('',#565,.T.);
#374=FACE_OUTER_BOUND('',#566,.T.);
#375=FACE_OUTER_BOUND('',#567,.T.);
#376=FACE_OUTER_BOUND('',#568,.T.);
#377=FACE_OUTER_BOUND('',#569,.T.);
#378=FACE_OUTER_BOUND('',#570,.T.);
#379=FACE_OUTER_BOUND('',#571,.T.);
#380=FACE_OUTER_BOUND('',#572,.T.);
#381=FACE_OUTER_BOUND('',#573,.T.);
#382=FACE_OUTER_BOUND('',#574,.T.);
#383=FACE_OUTER_BOUND('',#575,.T.);
#384=FACE_OUTER_BOUND('',#576,.T.);
#385=FACE_OUTER_BOUND('',#577,.T.);
#386=FACE_OUTER_BOUND('',#578,.T.);
#387=FACE_OUTER_BOUND('',#579,.T.);
#388=FACE_OUTER_BOUND('',#581,.T.);
#389=FACE_OUTER_BOUND('',#582,.T.);
#390=FACE_OUTER_BOUND('',#583,.T.);
#391=FACE_OUTER_BOUND('',#584,.T.);
#392=FACE_OUTER_BOUND('',#585,.T.);
#393=FACE_OUTER_BOUND('',#586,.T.);
#394=FACE_OUTER_BOUND('',#587,.T.);
#395=FACE_OUTER_BOUND('',#588,.T.);
#396=FACE_OUTER_BOUND('',#589,.T.);
#397=FACE_OUTER_BOUND('',#591,.T.);
#398=FACE_OUTER_BOUND('',#592,.T.);
#399=FACE_OUTER_BOUND('',#594,.T.);
#400=FACE_OUTER_BOUND('',#595,.T.);
#401=FACE_OUTER_BOUND('',#596,.T.);
#402=FACE_OUTER_BOUND('',#597,.T.);
#403=FACE_OUTER_BOUND('',#598,.T.);
#404=FACE_OUTER_BOUND('',#600,.T.);
#405=FACE_OUTER_BOUND('',#602,.T.);
#406=FACE_OUTER_BOUND('',#604,.T.);
#407=FACE_OUTER_BOUND('',#605,.T.);
#408=FACE_OUTER_BOUND('',#606,.T.);
#409=FACE_OUTER_BOUND('',#607,.T.);
#410=FACE_OUTER_BOUND('',#608,.T.);
#411=FACE_OUTER_BOUND('',#609,.T.);
#412=FACE_OUTER_BOUND('',#610,.T.);
#413=FACE_OUTER_BOUND('',#611,.T.);
#414=FACE_OUTER_BOUND('',#612,.T.);
#415=FACE_OUTER_BOUND('',#613,.T.);
#416=FACE_OUTER_BOUND('',#614,.T.);
#417=FACE_OUTER_BOUND('',#615,.T.);
#418=FACE_OUTER_BOUND('',#616,.T.);
#419=FACE_OUTER_BOUND('',#617,.T.);
#420=FACE_OUTER_BOUND('',#618,.T.);
#421=FACE_OUTER_BOUND('',#619,.T.);
#422=FACE_OUTER_BOUND('',#620,.T.);
#423=FACE_OUTER_BOUND('',#621,.T.);
#424=FACE_OUTER_BOUND('',#622,.T.);
#425=FACE_OUTER_BOUND('',#623,.T.);
#426=FACE_OUTER_BOUND('',#624,.T.);
#427=FACE_OUTER_BOUND('',#625,.T.);
#428=FACE_OUTER_BOUND('',#626,.T.);
#429=FACE_OUTER_BOUND('',#627,.T.);
#430=FACE_OUTER_BOUND('',#628,.T.);
#431=FACE_OUTER_BOUND('',#629,.T.);
#432=FACE_OUTER_BOUND('',#630,.T.);
#433=FACE_OUTER_BOUND('',#631,.T.);
#434=FACE_OUTER_BOUND('',#632,.T.);
#435=FACE_OUTER_BOUND('',#633,.T.);
#436=FACE_OUTER_BOUND('',#634,.T.);
#437=FACE_OUTER_BOUND('',#635,.T.);
#438=FACE_OUTER_BOUND('',#636,.T.);
#439=FACE_OUTER_BOUND('',#637,.T.);
#440=FACE_OUTER_BOUND('',#638,.T.);
#441=FACE_OUTER_BOUND('',#639,.T.);
#442=FACE_OUTER_BOUND('',#640,.T.);
#443=FACE_OUTER_BOUND('',#641,.T.);
#444=FACE_OUTER_BOUND('',#642,.T.);
#445=FACE_OUTER_BOUND('',#643,.T.);
#446=FACE_OUTER_BOUND('',#644,.T.);
#447=FACE_OUTER_BOUND('',#645,.T.);
#448=FACE_OUTER_BOUND('',#646,.T.);
#449=FACE_OUTER_BOUND('',#647,.T.);
#450=FACE_OUTER_BOUND('',#648,.T.);
#451=FACE_OUTER_BOUND('',#649,.T.);
#452=FACE_OUTER_BOUND('',#650,.T.);
#453=FACE_OUTER_BOUND('',#651,.T.);
#454=FACE_OUTER_BOUND('',#652,.T.);
#455=FACE_OUTER_BOUND('',#653,.T.);
#456=FACE_OUTER_BOUND('',#654,.T.);
#457=FACE_OUTER_BOUND('',#655,.T.);
#458=FACE_OUTER_BOUND('',#656,.T.);
#459=FACE_OUTER_BOUND('',#657,.T.);
#460=FACE_OUTER_BOUND('',#658,.T.);
#461=FACE_OUTER_BOUND('',#659,.T.);
#462=FACE_OUTER_BOUND('',#660,.T.);
#463=FACE_OUTER_BOUND('',#661,.T.);
#464=FACE_OUTER_BOUND('',#662,.T.);
#465=FACE_OUTER_BOUND('',#663,.T.);
#466=FACE_OUTER_BOUND('',#664,.T.);
#467=FACE_OUTER_BOUND('',#665,.T.);
#468=FACE_OUTER_BOUND('',#666,.T.);
#469=FACE_OUTER_BOUND('',#667,.T.);
#470=FACE_OUTER_BOUND('',#668,.T.);
#471=FACE_OUTER_BOUND('',#669,.T.);
#472=FACE_OUTER_BOUND('',#670,.T.);
#473=FACE_OUTER_BOUND('',#671,.T.);
#474=FACE_OUTER_BOUND('',#672,.T.);
#475=FACE_OUTER_BOUND('',#674,.T.);
#476=FACE_OUTER_BOUND('',#676,.T.);
#477=FACE_OUTER_BOUND('',#677,.T.);
#478=FACE_OUTER_BOUND('',#678,.T.);
#479=FACE_OUTER_BOUND('',#679,.T.);
#480=FACE_OUTER_BOUND('',#680,.T.);
#481=FACE_OUTER_BOUND('',#681,.T.);
#482=FACE_OUTER_BOUND('',#682,.T.);
#483=FACE_OUTER_BOUND('',#683,.T.);
#484=FACE_OUTER_BOUND('',#684,.T.);
#485=FACE_OUTER_BOUND('',#685,.T.);
#486=FACE_OUTER_BOUND('',#686,.T.);
#487=FACE_OUTER_BOUND('',#688,.T.);
#488=FACE_OUTER_BOUND('',#690,.T.);
#489=FACE_OUTER_BOUND('',#692,.T.);
#490=FACE_OUTER_BOUND('',#693,.T.);
#491=FACE_OUTER_BOUND('',#694,.T.);
#492=FACE_OUTER_BOUND('',#695,.T.);
#493=FACE_OUTER_BOUND('',#696,.T.);
#494=FACE_OUTER_BOUND('',#698,.T.);
#495=FACE_OUTER_BOUND('',#700,.T.);
#496=FACE_OUTER_BOUND('',#702,.T.);
#497=FACE_OUTER_BOUND('',#703,.T.);
#498=FACE_OUTER_BOUND('',#704,.T.);
#499=FACE_OUTER_BOUND('',#705,.T.);
#500=FACE_OUTER_BOUND('',#706,.T.);
#501=FACE_OUTER_BOUND('',#707,.T.);
#502=FACE_OUTER_BOUND('',#708,.T.);
#503=FACE_OUTER_BOUND('',#709,.T.);
#504=FACE_OUTER_BOUND('',#710,.T.);
#505=FACE_OUTER_BOUND('',#711,.T.);
#506=FACE_OUTER_BOUND('',#712,.T.);
#507=FACE_OUTER_BOUND('',#713,.T.);
#508=FACE_OUTER_BOUND('',#714,.T.);
#509=FACE_OUTER_BOUND('',#715,.T.);
#510=FACE_OUTER_BOUND('',#718,.T.);
#511=FACE_OUTER_BOUND('',#721,.T.);
#512=FACE_OUTER_BOUND('',#722,.T.);
#513=FACE_OUTER_BOUND('',#723,.T.);
#514=FACE_OUTER_BOUND('',#724,.T.);
#515=FACE_OUTER_BOUND('',#727,.T.);
#516=FACE_OUTER_BOUND('',#730,.T.);
#517=FACE_OUTER_BOUND('',#731,.T.);
#518=FACE_OUTER_BOUND('',#732,.T.);
#519=FACE_OUTER_BOUND('',#733,.T.);
#520=FACE_OUTER_BOUND('',#734,.T.);
#521=FACE_OUTER_BOUND('',#735,.T.);
#522=FACE_OUTER_BOUND('',#736,.T.);
#523=FACE_OUTER_BOUND('',#737,.T.);
#524=FACE_OUTER_BOUND('',#738,.T.);
#525=FACE_OUTER_BOUND('',#739,.T.);
#526=FACE_OUTER_BOUND('',#740,.T.);
#527=FACE_OUTER_BOUND('',#741,.T.);
#528=FACE_OUTER_BOUND('',#742,.T.);
#529=FACE_OUTER_BOUND('',#743,.T.);
#530=FACE_OUTER_BOUND('',#744,.T.);
#531=FACE_OUTER_BOUND('',#745,.T.);
#532=FACE_OUTER_BOUND('',#746,.T.);
#533=FACE_OUTER_BOUND('',#747,.T.);
#534=FACE_OUTER_BOUND('',#748,.T.);
#535=FACE_OUTER_BOUND('',#750,.T.);
#536=FACE_OUTER_BOUND('',#752,.T.);
#537=FACE_OUTER_BOUND('',#753,.T.);
#538=FACE_OUTER_BOUND('',#754,.T.);
#539=FACE_OUTER_BOUND('',#755,.T.);
#540=FACE_OUTER_BOUND('',#756,.T.);
#541=FACE_OUTER_BOUND('',#757,.T.);
#542=FACE_OUTER_BOUND('',#758,.T.);
#543=FACE_OUTER_BOUND('',#759,.T.);
#544=FACE_OUTER_BOUND('',#760,.T.);
#545=FACE_OUTER_BOUND('',#761,.T.);
#546=FACE_OUTER_BOUND('',#762,.T.);
#547=FACE_OUTER_BOUND('',#763,.T.);
#548=FACE_OUTER_BOUND('',#764,.T.);
#549=FACE_OUTER_BOUND('',#765,.T.);
#550=FACE_OUTER_BOUND('',#766,.T.);
#551=FACE_OUTER_BOUND('',#767,.T.);
#552=FACE_OUTER_BOUND('',#768,.T.);
#553=FACE_OUTER_BOUND('',#770,.T.);
#554=FACE_OUTER_BOUND('',#771,.T.);
#555=EDGE_LOOP('',(#2197,#2198,#2199,#2200));
#556=EDGE_LOOP('',(#2201,#2202,#2203,#2204));
#557=EDGE_LOOP('',(#2205,#2206,#2207,#2208,#2209,#2210,#2211,#2212));
#558=EDGE_LOOP('',(#2213));
#559=EDGE_LOOP('',(#2214,#2215,#2216,#2217));
#560=EDGE_LOOP('',(#2218,#2219,#2220,#2221,#2222,#2223,#2224,#2225));
#561=EDGE_LOOP('',(#2226));
#562=EDGE_LOOP('',(#2227,#2228,#2229,#2230));
#563=EDGE_LOOP('',(#2231,#2232,#2233,#2234,#2235,#2236));
#564=EDGE_LOOP('',(#2237,#2238,#2239,#2240));
#565=EDGE_LOOP('',(#2241,#2242,#2243,#2244,#2245,#2246));
#566=EDGE_LOOP('',(#2247,#2248,#2249,#2250));
#567=EDGE_LOOP('',(#2251,#2252,#2253,#2254));
#568=EDGE_LOOP('',(#2255,#2256,#2257,#2258,#2259,#2260));
#569=EDGE_LOOP('',(#2261,#2262,#2263,#2264));
#570=EDGE_LOOP('',(#2265,#2266,#2267,#2268,#2269,#2270));
#571=EDGE_LOOP('',(#2271,#2272,#2273,#2274));
#572=EDGE_LOOP('',(#2275,#2276,#2277,#2278));
#573=EDGE_LOOP('',(#2279,#2280,#2281,#2282));
#574=EDGE_LOOP('',(#2283,#2284,#2285,#2286));
#575=EDGE_LOOP('',(#2287,#2288,#2289,#2290));
#576=EDGE_LOOP('',(#2291,#2292,#2293,#2294));
#577=EDGE_LOOP('',(#2295,#2296,#2297,#2298,#2299,#2300,#2301,#2302,#2303,
#2304,#2305,#2306));
#578=EDGE_LOOP('',(#2307,#2308,#2309,#2310));
#579=EDGE_LOOP('',(#2311,#2312,#2313,#2314,#2315,#2316,#2317,#2318,#2319,
#2320,#2321,#2322));
#580=EDGE_LOOP('',(#2323));
#581=EDGE_LOOP('',(#2324,#2325,#2326,#2327));
#582=EDGE_LOOP('',(#2328,#2329,#2330,#2331));
#583=EDGE_LOOP('',(#2332,#2333,#2334,#2335,#2336,#2337,#2338,#2339));
#584=EDGE_LOOP('',(#2340,#2341,#2342,#2343,#2344,#2345,#2346,#2347,#2348,
#2349,#2350,#2351));
#585=EDGE_LOOP('',(#2352,#2353,#2354,#2355));
#586=EDGE_LOOP('',(#2356,#2357,#2358,#2359));
#587=EDGE_LOOP('',(#2360,#2361,#2362,#2363));
#588=EDGE_LOOP('',(#2364,#2365,#2366,#2367));
#589=EDGE_LOOP('',(#2368,#2369,#2370,#2371,#2372,#2373,#2374,#2375));
#590=EDGE_LOOP('',(#2376));
#591=EDGE_LOOP('',(#2377,#2378,#2379,#2380));
#592=EDGE_LOOP('',(#2381,#2382,#2383,#2384,#2385,#2386,#2387,#2388,#2389,
#2390,#2391,#2392,#2393,#2394,#2395,#2396));
#593=EDGE_LOOP('',(#2397));
#594=EDGE_LOOP('',(#2398,#2399,#2400,#2401));
#595=EDGE_LOOP('',(#2402,#2403,#2404,#2405));
#596=EDGE_LOOP('',(#2406,#2407,#2408,#2409));
#597=EDGE_LOOP('',(#2410,#2411,#2412,#2413));
#598=EDGE_LOOP('',(#2414,#2415,#2416,#2417,#2418,#2419,#2420,#2421,#2422,
#2423,#2424,#2425));
#599=EDGE_LOOP('',(#2426));
#600=EDGE_LOOP('',(#2427,#2428,#2429,#2430,#2431,#2432,#2433,#2434,#2435,
#2436,#2437,#2438));
#601=EDGE_LOOP('',(#2439));
#602=EDGE_LOOP('',(#2440,#2441,#2442,#2443,#2444,#2445,#2446,#2447));
#603=EDGE_LOOP('',(#2448));
#604=EDGE_LOOP('',(#2449,#2450,#2451,#2452));
#605=EDGE_LOOP('',(#2453,#2454,#2455,#2456));
#606=EDGE_LOOP('',(#2457,#2458,#2459,#2460));
#607=EDGE_LOOP('',(#2461,#2462,#2463,#2464));
#608=EDGE_LOOP('',(#2465,#2466,#2467,#2468));
#609=EDGE_LOOP('',(#2469,#2470,#2471,#2472));
#610=EDGE_LOOP('',(#2473,#2474,#2475,#2476));
#611=EDGE_LOOP('',(#2477,#2478,#2479,#2480));
#612=EDGE_LOOP('',(#2481,#2482,#2483,#2484));
#613=EDGE_LOOP('',(#2485,#2486,#2487,#2488));
#614=EDGE_LOOP('',(#2489,#2490,#2491,#2492));
#615=EDGE_LOOP('',(#2493,#2494,#2495,#2496));
#616=EDGE_LOOP('',(#2497,#2498,#2499,#2500));
#617=EDGE_LOOP('',(#2501,#2502,#2503,#2504));
#618=EDGE_LOOP('',(#2505,#2506,#2507,#2508));
#619=EDGE_LOOP('',(#2509,#2510,#2511,#2512));
#620=EDGE_LOOP('',(#2513,#2514,#2515,#2516));
#621=EDGE_LOOP('',(#2517,#2518,#2519,#2520));
#622=EDGE_LOOP('',(#2521,#2522,#2523,#2524));
#623=EDGE_LOOP('',(#2525,#2526,#2527,#2528));
#624=EDGE_LOOP('',(#2529,#2530,#2531,#2532));
#625=EDGE_LOOP('',(#2533,#2534,#2535,#2536));
#626=EDGE_LOOP('',(#2537,#2538,#2539,#2540));
#627=EDGE_LOOP('',(#2541,#2542,#2543,#2544));
#628=EDGE_LOOP('',(#2545,#2546,#2547,#2548));
#629=EDGE_LOOP('',(#2549,#2550,#2551,#2552));
#630=EDGE_LOOP('',(#2553,#2554,#2555,#2556));
#631=EDGE_LOOP('',(#2557,#2558,#2559,#2560));
#632=EDGE_LOOP('',(#2561,#2562,#2563,#2564));
#633=EDGE_LOOP('',(#2565,#2566,#2567,#2568));
#634=EDGE_LOOP('',(#2569,#2570,#2571,#2572));
#635=EDGE_LOOP('',(#2573,#2574,#2575,#2576));
#636=EDGE_LOOP('',(#2577,#2578,#2579,#2580));
#637=EDGE_LOOP('',(#2581,#2582,#2583,#2584));
#638=EDGE_LOOP('',(#2585,#2586,#2587,#2588));
#639=EDGE_LOOP('',(#2589,#2590,#2591,#2592));
#640=EDGE_LOOP('',(#2593,#2594,#2595));
#641=EDGE_LOOP('',(#2596,#2597,#2598,#2599,#2600,#2601));
#642=EDGE_LOOP('',(#2602,#2603,#2604,#2605));
#643=EDGE_LOOP('',(#2606,#2607,#2608,#2609));
#644=EDGE_LOOP('',(#2610,#2611,#2612,#2613));
#645=EDGE_LOOP('',(#2614,#2615,#2616,#2617));
#646=EDGE_LOOP('',(#2618,#2619,#2620,#2621));
#647=EDGE_LOOP('',(#2622,#2623,#2624,#2625));
#648=EDGE_LOOP('',(#2626,#2627,#2628,#2629));
#649=EDGE_LOOP('',(#2630,#2631,#2632,#2633));
#650=EDGE_LOOP('',(#2634,#2635,#2636,#2637));
#651=EDGE_LOOP('',(#2638,#2639,#2640,#2641));
#652=EDGE_LOOP('',(#2642,#2643,#2644,#2645));
#653=EDGE_LOOP('',(#2646,#2647,#2648,#2649));
#654=EDGE_LOOP('',(#2650,#2651,#2652,#2653));
#655=EDGE_LOOP('',(#2654,#2655,#2656,#2657));
#656=EDGE_LOOP('',(#2658,#2659,#2660,#2661));
#657=EDGE_LOOP('',(#2662,#2663,#2664,#2665));
#658=EDGE_LOOP('',(#2666,#2667,#2668,#2669));
#659=EDGE_LOOP('',(#2670,#2671,#2672,#2673));
#660=EDGE_LOOP('',(#2674,#2675,#2676,#2677));
#661=EDGE_LOOP('',(#2678,#2679,#2680,#2681));
#662=EDGE_LOOP('',(#2682,#2683,#2684,#2685));
#663=EDGE_LOOP('',(#2686,#2687,#2688,#2689));
#664=EDGE_LOOP('',(#2690,#2691,#2692,#2693));
#665=EDGE_LOOP('',(#2694,#2695,#2696,#2697));
#666=EDGE_LOOP('',(#2698,#2699,#2700,#2701,#2702,#2703,#2704,#2705));
#667=EDGE_LOOP('',(#2706,#2707,#2708,#2709,#2710));
#668=EDGE_LOOP('',(#2711,#2712,#2713,#2714));
#669=EDGE_LOOP('',(#2715,#2716,#2717,#2718));
#670=EDGE_LOOP('',(#2719,#2720,#2721,#2722,#2723));
#671=EDGE_LOOP('',(#2724));
#672=EDGE_LOOP('',(#2725));
#673=EDGE_LOOP('',(#2726));
#674=EDGE_LOOP('',(#2727));
#675=EDGE_LOOP('',(#2728));
#676=EDGE_LOOP('',(#2729,#2730));
#677=EDGE_LOOP('',(#2731,#2732,#2733,#2734));
#678=EDGE_LOOP('',(#2735,#2736,#2737,#2738));
#679=EDGE_LOOP('',(#2739,#2740,#2741,#2742,#2743,#2744,#2745,#2746,#2747,
#2748,#2749,#2750,#2751,#2752,#2753,#2754,#2755,#2756,#2757,#2758,#2759,
#2760,#2761,#2762,#2763,#2764,#2765,#2766,#2767,#2768,#2769,#2770,#2771,
#2772,#2773,#2774,#2775,#2776,#2777,#2778,#2779,#2780,#2781,#2782,#2783,
#2784,#2785,#2786,#2787,#2788,#2789,#2790,#2791,#2792,#2793,#2794,#2795,
#2796));
#680=EDGE_LOOP('',(#2797,#2798,#2799,#2800));
#681=EDGE_LOOP('',(#2801,#2802,#2803,#2804,#2805,#2806,#2807,#2808,#2809,
#2810,#2811,#2812,#2813,#2814,#2815,#2816,#2817,#2818,#2819,#2820,#2821,
#2822,#2823,#2824,#2825,#2826,#2827,#2828,#2829,#2830,#2831,#2832,#2833,
#2834,#2835,#2836,#2837,#2838,#2839,#2840,#2841,#2842,#2843,#2844,#2845,
#2846,#2847,#2848,#2849,#2850,#2851,#2852,#2853,#2854,#2855,#2856,#2857,
#2858));
#682=EDGE_LOOP('',(#2859,#2860,#2861,#2862));
#683=EDGE_LOOP('',(#2863,#2864,#2865,#2866,#2867));
#684=EDGE_LOOP('',(#2868,#2869,#2870,#2871,#2872));
#685=EDGE_LOOP('',(#2873,#2874,#2875,#2876));
#686=EDGE_LOOP('',(#2877));
#687=EDGE_LOOP('',(#2878));
#688=EDGE_LOOP('',(#2879));
#689=EDGE_LOOP('',(#2880));
#690=EDGE_LOOP('',(#2881));
#691=EDGE_LOOP('',(#2882));
#692=EDGE_LOOP('',(#2883,#2884,#2885,#2886));
#693=EDGE_LOOP('',(#2887,#2888,#2889,#2890,#2891));
#694=EDGE_LOOP('',(#2892,#2893,#2894,#2895));
#695=EDGE_LOOP('',(#2896,#2897,#2898,#2899,#2900,#2901,#2902));
#696=EDGE_LOOP('',(#2903,#2904,#2905,#2906));
#697=EDGE_LOOP('',(#2907));
#698=EDGE_LOOP('',(#2908,#2909,#2910,#2911,#2912,#2913));
#699=EDGE_LOOP('',(#2914));
#700=EDGE_LOOP('',(#2915,#2916,#2917,#2918,#2919,#2920));
#701=EDGE_LOOP('',(#2921));
#702=EDGE_LOOP('',(#2922,#2923,#2924,#2925));
#703=EDGE_LOOP('',(#2926,#2927,#2928,#2929,#2930));
#704=EDGE_LOOP('',(#2931,#2932,#2933,#2934));
#705=EDGE_LOOP('',(#2935,#2936,#2937,#2938));
#706=EDGE_LOOP('',(#2939,#2940,#2941,#2942));
#707=EDGE_LOOP('',(#2943,#2944,#2945,#2946));
#708=EDGE_LOOP('',(#2947,#2948,#2949,#2950));
#709=EDGE_LOOP('',(#2951,#2952,#2953,#2954));
#710=EDGE_LOOP('',(#2955,#2956,#2957,#2958,#2959,#2960,#2961,#2962));
#711=EDGE_LOOP('',(#2963,#2964,#2965,#2966));
#712=EDGE_LOOP('',(#2967,#2968,#2969,#2970,#2971,#2972,#2973,#2974));
#713=EDGE_LOOP('',(#2975,#2976,#2977,#2978));
#714=EDGE_LOOP('',(#2979,#2980,#2981,#2982));
#715=EDGE_LOOP('',(#2983,#2984,#2985,#2986,#2987,#2988));
#716=EDGE_LOOP('',(#2989));
#717=EDGE_LOOP('',(#2990));
#718=EDGE_LOOP('',(#2991,#2992,#2993,#2994,#2995,#2996));
#719=EDGE_LOOP('',(#2997));
#720=EDGE_LOOP('',(#2998));
#721=EDGE_LOOP('',(#2999,#3000,#3001,#3002));
#722=EDGE_LOOP('',(#3003,#3004,#3005,#3006));
#723=EDGE_LOOP('',(#3007,#3008,#3009,#3010));
#724=EDGE_LOOP('',(#3011,#3012,#3013,#3014,#3015,#3016));
#725=EDGE_LOOP('',(#3017));
#726=EDGE_LOOP('',(#3018));
#727=EDGE_LOOP('',(#3019,#3020,#3021,#3022,#3023,#3024));
#728=EDGE_LOOP('',(#3025));
#729=EDGE_LOOP('',(#3026));
#730=EDGE_LOOP('',(#3027,#3028,#3029,#3030));
#731=EDGE_LOOP('',(#3031,#3032,#3033,#3034,#3035));
#732=EDGE_LOOP('',(#3036,#3037,#3038));
#733=EDGE_LOOP('',(#3039,#3040,#3041,#3042,#3043));
#734=EDGE_LOOP('',(#3044,#3045));
#735=EDGE_LOOP('',(#3046,#3047,#3048));
#736=EDGE_LOOP('',(#3049,#3050,#3051,#3052,#3053));
#737=EDGE_LOOP('',(#3054,#3055,#3056,#3057,#3058,#3059));
#738=EDGE_LOOP('',(#3060,#3061,#3062,#3063));
#739=EDGE_LOOP('',(#3064,#3065,#3066,#3067,#3068,#3069,#3070,#3071,#3072,
#3073,#3074,#3075));
#740=EDGE_LOOP('',(#3076,#3077,#3078,#3079,#3080));
#741=EDGE_LOOP('',(#3081,#3082,#3083,#3084,#3085));
#742=EDGE_LOOP('',(#3086,#3087,#3088,#3089,#3090));
#743=EDGE_LOOP('',(#3091,#3092,#3093,#3094,#3095));
#744=EDGE_LOOP('',(#3096,#3097,#3098,#3099,#3100));
#745=EDGE_LOOP('',(#3101,#3102,#3103,#3104,#3105));
#746=EDGE_LOOP('',(#3106,#3107,#3108,#3109,#3110));
#747=EDGE_LOOP('',(#3111,#3112,#3113,#3114,#3115));
#748=EDGE_LOOP('',(#3116,#3117,#3118,#3119,#3120,#3121));
#749=EDGE_LOOP('',(#3122));
#750=EDGE_LOOP('',(#3123));
#751=EDGE_LOOP('',(#3124));
#752=EDGE_LOOP('',(#3125,#3126,#3127));
#753=EDGE_LOOP('',(#3128,#3129,#3130));
#754=EDGE_LOOP('',(#3131,#3132,#3133));
#755=EDGE_LOOP('',(#3134,#3135,#3136));
#756=EDGE_LOOP('',(#3137,#3138,#3139));
#757=EDGE_LOOP('',(#3140,#3141,#3142));
#758=EDGE_LOOP('',(#3143,#3144,#3145,#3146));
#759=EDGE_LOOP('',(#3147,#3148,#3149,#3150));
#760=EDGE_LOOP('',(#3151,#3152,#3153,#3154,#3155));
#761=EDGE_LOOP('',(#3156,#3157,#3158,#3159,#3160));
#762=EDGE_LOOP('',(#3161,#3162,#3163,#3164));
#763=EDGE_LOOP('',(#3165,#3166,#3167,#3168));
#764=EDGE_LOOP('',(#3169,#3170,#3171,#3172));
#765=EDGE_LOOP('',(#3173,#3174,#3175,#3176));
#766=EDGE_LOOP('',(#3177,#3178,#3179,#3180));
#767=EDGE_LOOP('',(#3181));
#768=EDGE_LOOP('',(#3182));
#769=EDGE_LOOP('',(#3183));
#770=EDGE_LOOP('',(#3184));
#771=EDGE_LOOP('',(#3185));
#772=EDGE_LOOP('',(#3186));
#773=LINE('',#4707,#1030);
#774=LINE('',#4714,#1031);
#775=LINE('',#4717,#1032);
#776=LINE('',#4720,#1033);
#777=LINE('',#4722,#1034);
#778=LINE('',#4724,#1035);
#779=LINE('',#4728,#1036);
#780=LINE('',#4730,#1037);
#781=LINE('',#4731,#1038);
#782=LINE('',#4734,#1039);
#783=LINE('',#4737,#1040);
#784=LINE('',#4740,#1041);
#785=LINE('',#4742,#1042);
#786=LINE('',#4743,#1043);
#787=LINE('',#4745,#1044);
#788=LINE('',#4747,#1045);
#789=LINE('',#4748,#1046);
#790=LINE('',#4751,#1047);
#791=LINE('',#4753,#1048);
#792=LINE('',#4754,#1049);
#793=LINE('',#4757,#1050);
#794=LINE('',#4758,#1051);
#795=LINE('',#4761,#1052);
#796=LINE('',#4762,#1053);
#797=LINE('',#4764,#1054);
#798=LINE('',#4768,#1055);
#799=LINE('',#4770,#1056);
#800=LINE('',#4771,#1057);
#801=LINE('',#4774,#1058);
#802=LINE('',#4775,#1059);
#803=LINE('',#4778,#1060);
#804=LINE('',#4779,#1061);
#805=LINE('',#4781,#1062);
#806=LINE('',#4788,#1063);
#807=LINE('',#4794,#1064);
#808=LINE('',#4800,#1065);
#809=LINE('',#4807,#1066);
#810=LINE('',#4810,#1067);
#811=LINE('',#4816,#1068);
#812=LINE('',#4819,#1069);
#813=LINE('',#4823,#1070);
#814=LINE('',#4825,#1071);
#815=LINE('',#4827,#1072);
#816=LINE('',#4829,#1073);
#817=LINE('',#4831,#1074);
#818=LINE('',#4833,#1075);
#819=LINE('',#4835,#1076);
#820=LINE('',#4837,#1077);
#821=LINE('',#4839,#1078);
#822=LINE('',#4841,#1079);
#823=LINE('',#4843,#1080);
#824=LINE('',#4844,#1081);
#825=LINE('',#4847,#1082);
#826=LINE('',#4849,#1083);
#827=LINE('',#4850,#1084);
#828=LINE('',#4853,#1085);
#829=LINE('',#4855,#1086);
#830=LINE('',#4857,#1087);
#831=LINE('',#4861,#1088);
#832=LINE('',#4863,#1089);
#833=LINE('',#4865,#1090);
#834=LINE('',#4867,#1091);
#835=LINE('',#4869,#1092);
#836=LINE('',#4871,#1093);
#837=LINE('',#4872,#1094);
#838=LINE('',#4875,#1095);
#839=LINE('',#4876,#1096);
#840=LINE('',#4879,#1097);
#841=LINE('',#4881,#1098);
#842=LINE('',#4882,#1099);
#843=LINE('',#4886,#1100);
#844=LINE('',#4888,#1101);
#845=LINE('',#4889,#1102);
#846=LINE('',#4891,#1103);
#847=LINE('',#4893,#1104);
#848=LINE('',#4895,#1105);
#849=LINE('',#4896,#1106);
#850=LINE('',#4899,#1107);
#851=LINE('',#4901,#1108);
#852=LINE('',#4903,#1109);
#853=LINE('',#4905,#1110);
#854=LINE('',#4907,#1111);
#855=LINE('',#4909,#1112);
#856=LINE('',#4910,#1113);
#857=LINE('',#4911,#1114);
#858=LINE('',#4913,#1115);
#859=LINE('',#4914,#1116);
#860=LINE('',#4917,#1117);
#861=LINE('',#4919,#1118);
#862=LINE('',#4920,#1119);
#863=LINE('',#4922,#1120);
#864=LINE('',#4923,#1121);
#865=LINE('',#4926,#1122);
#866=LINE('',#4928,#1123);
#867=LINE('',#4929,#1124);
#868=LINE('',#4934,#1125);
#869=LINE('',#4936,#1126);
#870=LINE('',#4937,#1127);
#871=LINE('',#4939,#1128);
#872=LINE('',#4940,#1129);
#873=LINE('',#4942,#1130);
#874=LINE('',#4945,#1131);
#875=LINE('',#4951,#1132);
#876=LINE('',#4953,#1133);
#877=LINE('',#4955,#1134);
#878=LINE('',#4957,#1135);
#879=LINE('',#4959,#1136);
#880=LINE('',#4960,#1137);
#881=LINE('',#4961,#1138);
#882=LINE('',#4966,#1139);
#883=LINE('',#4968,#1140);
#884=LINE('',#4969,#1141);
#885=LINE('',#4971,#1142);
#886=LINE('',#4973,#1143);
#887=LINE('',#4975,#1144);
#888=LINE('',#4976,#1145);
#889=LINE('',#4977,#1146);
#890=LINE('',#4979,#1147);
#891=LINE('',#4982,#1148);
#892=LINE('',#4984,#1149);
#893=LINE('',#4986,#1150);
#894=LINE('',#4992,#1151);
#895=LINE('',#4998,#1152);
#896=LINE('',#5004,#1153);
#897=LINE('',#5011,#1154);
#898=LINE('',#5041,#1155);
#899=LINE('',#5071,#1156);
#900=LINE('',#5101,#1157);
#901=LINE('',#5131,#1158);
#902=LINE('',#5161,#1159);
#903=LINE('',#5191,#1160);
#904=LINE('',#5221,#1161);
#905=LINE('',#5251,#1162);
#906=LINE('',#5281,#1163);
#907=LINE('',#5311,#1164);
#908=LINE('',#5341,#1165);
#909=LINE('',#5371,#1166);
#910=LINE('',#5401,#1167);
#911=LINE('',#5431,#1168);
#912=LINE('',#5461,#1169);
#913=LINE('',#5491,#1170);
#914=LINE('',#5521,#1171);
#915=LINE('',#5551,#1172);
#916=LINE('',#5581,#1173);
#917=LINE('',#5611,#1174);
#918=LINE('',#5641,#1175);
#919=LINE('',#5671,#1176);
#920=LINE('',#5701,#1177);
#921=LINE('',#5731,#1178);
#922=LINE('',#5761,#1179);
#923=LINE('',#5791,#1180);
#924=LINE('',#5809,#1181);
#925=LINE('',#5848,#1182);
#926=LINE('',#5864,#1183);
#927=LINE('',#5940,#1184);
#928=LINE('',#6018,#1185);
#929=LINE('',#6096,#1186);
#930=LINE('',#6172,#1187);
#931=LINE('',#6248,#1188);
#932=LINE('',#6324,#1189);
#933=LINE('',#6402,#1190);
#934=LINE('',#6478,#1191);
#935=LINE('',#6556,#1192);
#936=LINE('',#6632,#1193);
#937=LINE('',#6708,#1194);
#938=LINE('',#6784,#1195);
#939=LINE('',#6860,#1196);
#940=LINE('',#6938,#1197);
#941=LINE('',#7016,#1198);
#942=LINE('',#7092,#1199);
#943=LINE('',#7168,#1200);
#944=LINE('',#7244,#1201);
#945=LINE('',#7322,#1202);
#946=LINE('',#7400,#1203);
#947=LINE('',#7476,#1204);
#948=LINE('',#7552,#1205);
#949=LINE('',#7628,#1206);
#950=LINE('',#7705,#1207);
#951=LINE('',#7724,#1208);
#952=LINE('',#7745,#1209);
#953=LINE('',#7869,#1210);
#954=LINE('',#7873,#1211);
#955=LINE('',#7881,#1212);
#956=LINE('',#7883,#1213);
#957=LINE('',#7884,#1214);
#958=LINE('',#7886,#1215);
#959=LINE('',#7887,#1216);
#960=LINE('',#9192,#1217);
#961=LINE('',#9200,#1218);
#962=LINE('',#9204,#1219);
#963=LINE('',#9210,#1220);
#964=LINE('',#9220,#1221);
#965=LINE('',#9227,#1222);
#966=LINE('',#9235,#1223);
#967=LINE('',#9238,#1224);
#968=LINE('',#9241,#1225);
#969=LINE('',#9242,#1226);
#970=LINE('',#9244,#1227);
#971=LINE('',#9245,#1228);
#972=LINE('',#9248,#1229);
#973=LINE('',#9250,#1230);
#974=LINE('',#9251,#1231);
#975=LINE('',#9256,#1232);
#976=LINE('',#9263,#1233);
#977=LINE('',#9265,#1234);
#978=LINE('',#9266,#1235);
#979=LINE('',#9274,#1236);
#980=LINE('',#9280,#1237);
#981=LINE('',#9286,#1238);
#982=LINE('',#9292,#1239);
#983=LINE('',#9299,#1240);
#984=LINE('',#9302,#1241);
#985=LINE('',#9306,#1242);
#986=LINE('',#9308,#1243);
#987=LINE('',#9310,#1244);
#988=LINE('',#9312,#1245);
#989=LINE('',#9314,#1246);
#990=LINE('',#9316,#1247);
#991=LINE('',#9318,#1248);
#992=LINE('',#9319,#1249);
#993=LINE('',#9322,#1250);
#994=LINE('',#9324,#1251);
#995=LINE('',#9325,#1252);
#996=LINE('',#9328,#1253);
#997=LINE('',#9330,#1254);
#998=LINE('',#9332,#1255);
#999=LINE('',#9334,#1256);
#1000=LINE('',#9336,#1257);
#1001=LINE('',#9338,#1258);
#1002=LINE('',#9339,#1259);
#1003=LINE('',#9341,#1260);
#1004=LINE('',#9342,#1261);
#1005=LINE('',#9344,#1262);
#1006=LINE('',#9345,#1263);
#1007=LINE('',#9348,#1264);
#1008=LINE('',#9350,#1265);
#1009=LINE('',#9353,#1266);
#1010=LINE('',#9355,#1267);
#1011=LINE('',#9356,#1268);
#1012=LINE('',#9359,#1269);
#1013=LINE('',#9361,#1270);
#1014=LINE('',#9362,#1271);
#1015=LINE('',#11566,#1272);
#1016=LINE('',#13282,#1273);
#1017=LINE('',#13290,#1274);
#1018=LINE('',#13296,#1275);
#1019=LINE('',#13303,#1276);
#1020=LINE('',#13397,#1277);
#1021=LINE('',#13401,#1278);
#1022=LINE('',#13441,#1279);
#1023=LINE('',#13452,#1280);
#1024=LINE('',#13500,#1281);
#1025=LINE('',#13548,#1282);
#1026=LINE('',#13596,#1283);
#1027=LINE('',#14035,#1284);
#1028=LINE('',#14041,#1285);
#1029=LINE('',#14047,#1286);
#1030=VECTOR('',#3872,30.);
#1031=VECTOR('',#3879,1000.);
#1032=VECTOR('',#3882,1000.);
#1033=VECTOR('',#3885,1000.);
#1034=VECTOR('',#3886,1000.);
#1035=VECTOR('',#3887,1000.);
#1036=VECTOR('',#3890,1000.);
#1037=VECTOR('',#3891,1000.);
#1038=VECTOR('',#3892,1000.);
#1039=VECTOR('',#3895,1000.);
#1040=VECTOR('',#3898,1000.);
#1041=VECTOR('',#3901,1000.);
#1042=VECTOR('',#3902,1000.);
#1043=VECTOR('',#3903,1000.);
#1044=VECTOR('',#3904,1000.);
#1045=VECTOR('',#3905,1000.);
#1046=VECTOR('',#3906,1000.);
#1047=VECTOR('',#3909,1000.);
#1048=VECTOR('',#3910,1000.);
#1049=VECTOR('',#3911,1000.);
#1050=VECTOR('',#3914,1000.);
#1051=VECTOR('',#3915,1000.);
#1052=VECTOR('',#3918,1000.);
#1053=VECTOR('',#3919,1000.);
#1054=VECTOR('',#3922,1000.);
#1055=VECTOR('',#3927,1000.);
#1056=VECTOR('',#3928,1000.);
#1057=VECTOR('',#3929,1000.);
#1058=VECTOR('',#3932,1000.);
#1059=VECTOR('',#3933,1000.);
#1060=VECTOR('',#3936,1000.);
#1061=VECTOR('',#3937,1000.);
#1062=VECTOR('',#3940,1000.);
#1063=VECTOR('',#3949,2.);
#1064=VECTOR('',#3956,6.);
#1065=VECTOR('',#3963,6.);
#1066=VECTOR('',#3970,1000.);
#1067=VECTOR('',#3973,1000.);
#1068=VECTOR('',#3978,1000.);
#1069=VECTOR('',#3981,1000.);
#1070=VECTOR('',#3984,1000.);
#1071=VECTOR('',#3985,1000.);
#1072=VECTOR('',#3986,1000.);
#1073=VECTOR('',#3987,1000.);
#1074=VECTOR('',#3988,1000.);
#1075=VECTOR('',#3989,1000.);
#1076=VECTOR('',#3990,1000.);
#1077=VECTOR('',#3991,1000.);
#1078=VECTOR('',#3992,1000.);
#1079=VECTOR('',#3993,1000.);
#1080=VECTOR('',#3994,1000.);
#1081=VECTOR('',#3995,1000.);
#1082=VECTOR('',#3998,1000.);
#1083=VECTOR('',#3999,1000.);
#1084=VECTOR('',#4000,1000.);
#1085=VECTOR('',#4003,1000.);
#1086=VECTOR('',#4004,1000.);
#1087=VECTOR('',#4005,1000.);
#1088=VECTOR('',#4008,1000.);
#1089=VECTOR('',#4009,1000.);
#1090=VECTOR('',#4010,1000.);
#1091=VECTOR('',#4011,1000.);
#1092=VECTOR('',#4012,1000.);
#1093=VECTOR('',#4013,1000.);
#1094=VECTOR('',#4014,1000.);
#1095=VECTOR('',#4017,1000.);
#1096=VECTOR('',#4018,1000.);
#1097=VECTOR('',#4021,1000.);
#1098=VECTOR('',#4022,1000.);
#1099=VECTOR('',#4023,1000.);
#1100=VECTOR('',#4026,1000.);
#1101=VECTOR('',#4027,1000.);
#1102=VECTOR('',#4028,1000.);
#1103=VECTOR('',#4029,1000.);
#1104=VECTOR('',#4030,1000.);
#1105=VECTOR('',#4031,1000.);
#1106=VECTOR('',#4032,1000.);
#1107=VECTOR('',#4035,1000.);
#1108=VECTOR('',#4036,1000.);
#1109=VECTOR('',#4037,1000.);
#1110=VECTOR('',#4038,1000.);
#1111=VECTOR('',#4039,1000.);
#1112=VECTOR('',#4040,1000.);
#1113=VECTOR('',#4041,1000.);
#1114=VECTOR('',#4042,1000.);
#1115=VECTOR('',#4045,1000.);
#1116=VECTOR('',#4046,1000.);
#1117=VECTOR('',#4049,1000.);
#1118=VECTOR('',#4050,1000.);
#1119=VECTOR('',#4051,1000.);
#1120=VECTOR('',#4054,1000.);
#1121=VECTOR('',#4055,1000.);
#1122=VECTOR('',#4058,1000.);
#1123=VECTOR('',#4059,1000.);
#1124=VECTOR('',#4060,1000.);
#1125=VECTOR('',#4067,1000.);
#1126=VECTOR('',#4068,1000.);
#1127=VECTOR('',#4069,1000.);
#1128=VECTOR('',#4072,1000.);
#1129=VECTOR('',#4073,1000.);
#1130=VECTOR('',#4076,1000.);
#1131=VECTOR('',#4081,1000.);
#1132=VECTOR('',#4088,1000.);
#1133=VECTOR('',#4091,1000.);
#1134=VECTOR('',#4092,1000.);
#1135=VECTOR('',#4093,1000.);
#1136=VECTOR('',#4094,1000.);
#1137=VECTOR('',#4095,1000.);
#1138=VECTOR('',#4096,1000.);
#1139=VECTOR('',#4101,1000.);
#1140=VECTOR('',#4102,1000.);
#1141=VECTOR('',#4103,1000.);
#1142=VECTOR('',#4104,1000.);
#1143=VECTOR('',#4105,1000.);
#1144=VECTOR('',#4106,1000.);
#1145=VECTOR('',#4107,1000.);
#1146=VECTOR('',#4108,1000.);
#1147=VECTOR('',#4111,1000.);
#1148=VECTOR('',#4116,1000.);
#1149=VECTOR('',#4119,1000.);
#1150=VECTOR('',#4122,1000.);
#1151=VECTOR('',#4133,1000.);
#1152=VECTOR('',#4140,5.75643035625);
#1153=VECTOR('',#4141,10.);
#1154=VECTOR('',#4144,5.75643035625);
#1155=VECTOR('',#4147,5.75643035625);
#1156=VECTOR('',#4150,5.75643035625);
#1157=VECTOR('',#4153,5.75643035625);
#1158=VECTOR('',#4156,5.75643035625);
#1159=VECTOR('',#4159,5.75643035625);
#1160=VECTOR('',#4162,5.75643035625);
#1161=VECTOR('',#4165,5.75643035625);
#1162=VECTOR('',#4168,5.75643035625);
#1163=VECTOR('',#4171,5.75643035625);
#1164=VECTOR('',#4174,5.75643035625);
#1165=VECTOR('',#4177,5.75643035625);
#1166=VECTOR('',#4180,5.75643035625);
#1167=VECTOR('',#4183,5.75643035625);
#1168=VECTOR('',#4186,5.75643035625);
#1169=VECTOR('',#4189,5.75643035625);
#1170=VECTOR('',#4192,5.75643035625);
#1171=VECTOR('',#4195,5.75643035625);
#1172=VECTOR('',#4198,5.75643035625);
#1173=VECTOR('',#4201,5.75643035625);
#1174=VECTOR('',#4204,5.75643035625);
#1175=VECTOR('',#4207,5.75643035625);
#1176=VECTOR('',#4210,5.75643035625);
#1177=VECTOR('',#4213,5.75643035625);
#1178=VECTOR('',#4216,5.75643035625);
#1179=VECTOR('',#4219,5.75643035625);
#1180=VECTOR('',#4222,6.);
#1181=VECTOR('',#4227,6.);
#1182=VECTOR('',#4230,1000.);
#1183=VECTOR('',#4233,6.);
#1184=VECTOR('',#4236,6.);
#1185=VECTOR('',#4239,6.);
#1186=VECTOR('',#4242,6.);
#1187=VECTOR('',#4245,6.);
#1188=VECTOR('',#4248,6.);
#1189=VECTOR('',#4251,6.);
#1190=VECTOR('',#4254,6.);
#1191=VECTOR('',#4257,6.);
#1192=VECTOR('',#4260,6.);
#1193=VECTOR('',#4263,6.);
#1194=VECTOR('',#4266,6.);
#1195=VECTOR('',#4269,6.);
#1196=VECTOR('',#4272,6.);
#1197=VECTOR('',#4275,6.);
#1198=VECTOR('',#4278,6.);
#1199=VECTOR('',#4281,6.);
#1200=VECTOR('',#4284,6.);
#1201=VECTOR('',#4287,6.);
#1202=VECTOR('',#4290,6.);
#1203=VECTOR('',#4293,6.);
#1204=VECTOR('',#4296,6.);
#1205=VECTOR('',#4299,6.);
#1206=VECTOR('',#4302,6.);
#1207=VECTOR('',#4307,6.);
#1208=VECTOR('',#4308,1000.);
#1209=VECTOR('',#4309,6.);
#1210=VECTOR('',#4326,9.);
#1211=VECTOR('',#4331,6.);
#1212=VECTOR('',#4344,1000.);
#1213=VECTOR('',#4345,1000.);
#1214=VECTOR('',#4346,1000.);
#1215=VECTOR('',#4349,10.);
#1216=VECTOR('',#4350,10.);
#1217=VECTOR('',#4359,15.);
#1218=VECTOR('',#4368,30.);
#1219=VECTOR('',#4373,30.);
#1220=VECTOR('',#4380,6.);
#1221=VECTOR('',#4395,2.);
#1222=VECTOR('',#4402,6.25);
#1223=VECTOR('',#4411,1000.);
#1224=VECTOR('',#4414,1000.);
#1225=VECTOR('',#4417,1000.);
#1226=VECTOR('',#4418,1000.);
#1227=VECTOR('',#4419,1000.);
#1228=VECTOR('',#4420,1000.);
#1229=VECTOR('',#4423,1000.);
#1230=VECTOR('',#4424,1000.);
#1231=VECTOR('',#4425,1000.);
#1232=VECTOR('',#4430,1000.);
#1233=VECTOR('',#4439,1000.);
#1234=VECTOR('',#4442,1000.);
#1235=VECTOR('',#4443,1000.);
#1236=VECTOR('',#4454,2.);
#1237=VECTOR('',#4461,2.);
#1238=VECTOR('',#4468,2.);
#1239=VECTOR('',#4475,2.);
#1240=VECTOR('',#4482,1000.);
#1241=VECTOR('',#4485,1000.);
#1242=VECTOR('',#4488,1000.);
#1243=VECTOR('',#4489,1000.);
#1244=VECTOR('',#4490,1000.);
#1245=VECTOR('',#4491,1000.);
#1246=VECTOR('',#4492,1000.);
#1247=VECTOR('',#4493,1000.);
#1248=VECTOR('',#4494,1000.);
#1249=VECTOR('',#4495,1000.);
#1250=VECTOR('',#4498,1000.);
#1251=VECTOR('',#4499,1000.);
#1252=VECTOR('',#4500,1000.);
#1253=VECTOR('',#4503,1000.);
#1254=VECTOR('',#4504,1000.);
#1255=VECTOR('',#4505,1000.);
#1256=VECTOR('',#4506,1000.);
#1257=VECTOR('',#4507,1000.);
#1258=VECTOR('',#4508,1000.);
#1259=VECTOR('',#4509,1000.);
#1260=VECTOR('',#4512,1000.);
#1261=VECTOR('',#4513,1000.);
#1262=VECTOR('',#4516,1000.);
#1263=VECTOR('',#4517,1000.);
#1264=VECTOR('',#4522,1000.);
#1265=VECTOR('',#4525,1000.);
#1266=VECTOR('',#4528,1000.);
#1267=VECTOR('',#4529,1000.);
#1268=VECTOR('',#4530,1000.);
#1269=VECTOR('',#4533,1000.);
#1270=VECTOR('',#4534,1000.);
#1271=VECTOR('',#4535,1000.);
#1272=VECTOR('',#4556,1000.);
#1273=VECTOR('',#4569,6.);
#1274=VECTOR('',#4578,6.);
#1275=VECTOR('',#4585,5.01);
#1276=VECTOR('',#4592,12.389406481562);
#1277=VECTOR('',#4603,5.1);
#1278=VECTOR('',#4606,1000.);
#1279=VECTOR('',#4607,1000.);
#1280=VECTOR('',#4610,1000.);
#1281=VECTOR('',#4613,1000.);
#1282=VECTOR('',#4616,1000.);
#1283=VECTOR('',#4619,1000.);
#1284=VECTOR('',#4656,3.);
#1285=VECTOR('',#4663,3.);
#1286=VECTOR('',#4670,1.9);
#1287=CIRCLE('',#3577,30.);
#1288=CIRCLE('',#3578,30.);
#1289=CIRCLE('',#3580,40.);
#1290=CIRCLE('',#3581,40.);
#1291=CIRCLE('',#3583,40.);
#1292=CIRCLE('',#3585,40.);
#1293=CIRCLE('',#3599,2.);
#1294=CIRCLE('',#3600,2.);
#1295=CIRCLE('',#3602,6.);
#1296=CIRCLE('',#3603,6.);
#1297=CIRCLE('',#3605,6.);
#1298=CIRCLE('',#3606,6.);
#1299=CIRCLE('',#3608,12.5);
#1300=CIRCLE('',#3609,12.5);
#1301=CIRCLE('',#3611,12.5);
#1302=CIRCLE('',#3612,12.5);
#1303=CIRCLE('',#3616,12.5);
#1304=CIRCLE('',#3626,12.5);
#1305=CIRCLE('',#3629,12.5);
#1306=CIRCLE('',#3635,10.);
#1307=CIRCLE('',#3637,10.);
#1308=CIRCLE('',#3639,12.5);
#1309=CIRCLE('',#3678,6.);
#1310=CIRCLE('',#3680,6.);
#1311=CIRCLE('',#3706,6.);
#1312=CIRCLE('',#3708,6.00000000000001);
#1313=CIRCLE('',#3709,26.5);
#1314=CIRCLE('',#3710,6.);
#1315=CIRCLE('',#3711,6.);
#1316=CIRCLE('',#3714,9.);
#1317=CIRCLE('',#3715,9.);
#1318=CIRCLE('',#3717,6.);
#1319=CIRCLE('',#3727,15.);
#1320=CIRCLE('',#3728,15.);
#1321=CIRCLE('',#3730,30.);
#1322=CIRCLE('',#3731,30.);
#1323=CIRCLE('',#3732,24.);
#1324=CIRCLE('',#3734,30.);
#1325=CIRCLE('',#3736,6.);
#1326=CIRCLE('',#3737,6.);
#1327=CIRCLE('',#3743,2.);
#1328=CIRCLE('',#3744,2.);
#1329=CIRCLE('',#3746,6.25);
#1330=CIRCLE('',#3747,6.25);
#1331=CIRCLE('',#3748,6.25);
#1332=CIRCLE('',#3750,11.25);
#1333=CIRCLE('',#3751,11.25);
#1334=CIRCLE('',#3755,3.);
#1335=CIRCLE('',#3756,5.);
#1336=CIRCLE('',#3758,3.);
#1337=CIRCLE('',#3759,5.);
#1338=CIRCLE('',#3765,2.);
#1339=CIRCLE('',#3766,2.);
#1340=CIRCLE('',#3768,2.);
#1341=CIRCLE('',#3769,2.);
#1342=CIRCLE('',#3771,2.);
#1343=CIRCLE('',#3772,2.);
#1344=CIRCLE('',#3774,2.);
#1345=CIRCLE('',#3775,2.);
#1346=CIRCLE('',#3777,4.);
#1347=CIRCLE('',#3778,4.);
#1348=CIRCLE('',#3790,4.);
#1349=CIRCLE('',#3792,4.);
#1350=CIRCLE('',#3795,0.499999999999983);
#1351=CIRCLE('',#3796,0.499999999999983);
#1352=CIRCLE('',#3798,0.499999999999983);
#1353=CIRCLE('',#3799,0.499999999999983);
#1354=CIRCLE('',#3804,6.);
#1355=CIRCLE('',#3805,6.);
#1356=CIRCLE('',#3806,6.);
#1357=CIRCLE('',#3808,5.1);
#1358=CIRCLE('',#3809,5.1);
#1359=CIRCLE('',#3811,5.1);
#1360=CIRCLE('',#3812,6.);
#1361=CIRCLE('',#3814,12.389406481562);
#1362=CIRCLE('',#3815,12.389406481562);
#1363=CIRCLE('',#3817,0.927982083713184);
#1364=CIRCLE('',#3818,12.0720179162868);
#1365=CIRCLE('',#3827,9.);
#1366=CIRCLE('',#3828,9.);
#1367=CIRCLE('',#3829,9.);
#1368=CIRCLE('',#3830,9.);
#1369=CIRCLE('',#3831,9.);
#1370=CIRCLE('',#3832,9.);
#1371=CIRCLE('',#3842,3.);
#1372=CIRCLE('',#3843,3.);
#1373=CIRCLE('',#3845,3.);
#1374=CIRCLE('',#3846,3.);
#1375=CIRCLE('',#3848,1.9);
#1376=CIRCLE('',#3849,1.9);
#1377=VERTEX_POINT('',#4704);
#1378=VERTEX_POINT('',#4706);
#1379=VERTEX_POINT('',#4710);
#1380=VERTEX_POINT('',#4711);
#1381=VERTEX_POINT('',#4713);
#1382=VERTEX_POINT('',#4715);
#1383=VERTEX_POINT('',#4719);
#1384=VERTEX_POINT('',#4721);
#1385=VERTEX_POINT('',#4723);
#1386=VERTEX_POINT('',#4725);
#1387=VERTEX_POINT('',#4727);
#1388=VERTEX_POINT('',#4729);
#1389=VERTEX_POINT('',#4733);
#1390=VERTEX_POINT('',#4735);
#1391=VERTEX_POINT('',#4739);
#1392=VERTEX_POINT('',#4741);
#1393=VERTEX_POINT('',#4744);
#1394=VERTEX_POINT('',#4746);
#1395=VERTEX_POINT('',#4750);
#1396=VERTEX_POINT('',#4752);
#1397=VERTEX_POINT('',#4756);
#1398=VERTEX_POINT('',#4760);
#1399=VERTEX_POINT('',#4767);
#1400=VERTEX_POINT('',#4769);
#1401=VERTEX_POINT('',#4773);
#1402=VERTEX_POINT('',#4777);
#1403=VERTEX_POINT('',#4785);
#1404=VERTEX_POINT('',#4787);
#1405=VERTEX_POINT('',#4791);
#1406=VERTEX_POINT('',#4793);
#1407=VERTEX_POINT('',#4797);
#1408=VERTEX_POINT('',#4799);
#1409=VERTEX_POINT('',#4803);
#1410=VERTEX_POINT('',#4804);
#1411=VERTEX_POINT('',#4806);
#1412=VERTEX_POINT('',#4808);
#1413=VERTEX_POINT('',#4812);
#1414=VERTEX_POINT('',#4813);
#1415=VERTEX_POINT('',#4815);
#1416=VERTEX_POINT('',#4817);
#1417=VERTEX_POINT('',#4821);
#1418=VERTEX_POINT('',#4822);
#1419=VERTEX_POINT('',#4824);
#1420=VERTEX_POINT('',#4826);
#1421=VERTEX_POINT('',#4828);
#1422=VERTEX_POINT('',#4830);
#1423=VERTEX_POINT('',#4832);
#1424=VERTEX_POINT('',#4834);
#1425=VERTEX_POINT('',#4836);
#1426=VERTEX_POINT('',#4838);
#1427=VERTEX_POINT('',#4840);
#1428=VERTEX_POINT('',#4842);
#1429=VERTEX_POINT('',#4846);
#1430=VERTEX_POINT('',#4848);
#1431=VERTEX_POINT('',#4852);
#1432=VERTEX_POINT('',#4854);
#1433=VERTEX_POINT('',#4856);
#1434=VERTEX_POINT('',#4858);
#1435=VERTEX_POINT('',#4860);
#1436=VERTEX_POINT('',#4862);
#1437=VERTEX_POINT('',#4864);
#1438=VERTEX_POINT('',#4866);
#1439=VERTEX_POINT('',#4868);
#1440=VERTEX_POINT('',#4870);
#1441=VERTEX_POINT('',#4874);
#1442=VERTEX_POINT('',#4878);
#1443=VERTEX_POINT('',#4880);
#1444=VERTEX_POINT('',#4884);
#1445=VERTEX_POINT('',#4885);
#1446=VERTEX_POINT('',#4887);
#1447=VERTEX_POINT('',#4890);
#1448=VERTEX_POINT('',#4892);
#1449=VERTEX_POINT('',#4894);
#1450=VERTEX_POINT('',#4898);
#1451=VERTEX_POINT('',#4900);
#1452=VERTEX_POINT('',#4902);
#1453=VERTEX_POINT('',#4904);
#1454=VERTEX_POINT('',#4906);
#1455=VERTEX_POINT('',#4908);
#1456=VERTEX_POINT('',#4916);
#1457=VERTEX_POINT('',#4918);
#1458=VERTEX_POINT('',#4925);
#1459=VERTEX_POINT('',#4927);
#1460=VERTEX_POINT('',#4933);
#1461=VERTEX_POINT('',#4935);
#1462=VERTEX_POINT('',#4949);
#1463=VERTEX_POINT('',#4950);
#1464=VERTEX_POINT('',#4954);
#1465=VERTEX_POINT('',#4956);
#1466=VERTEX_POINT('',#4958);
#1467=VERTEX_POINT('',#4963);
#1468=VERTEX_POINT('',#4965);
#1469=VERTEX_POINT('',#4967);
#1470=VERTEX_POINT('',#4970);
#1471=VERTEX_POINT('',#4972);
#1472=VERTEX_POINT('',#4974);
#1473=VERTEX_POINT('',#4996);
#1474=VERTEX_POINT('',#4997);
#1475=VERTEX_POINT('',#4999);
#1476=VERTEX_POINT('',#5003);
#1477=VERTEX_POINT('',#5009);
#1478=VERTEX_POINT('',#5010);
#1479=VERTEX_POINT('',#5039);
#1480=VERTEX_POINT('',#5040);
#1481=VERTEX_POINT('',#5069);
#1482=VERTEX_POINT('',#5070);
#1483=VERTEX_POINT('',#5099);
#1484=VERTEX_POINT('',#5100);
#1485=VERTEX_POINT('',#5129);
#1486=VERTEX_POINT('',#5130);
#1487=VERTEX_POINT('',#5159);
#1488=VERTEX_POINT('',#5160);
#1489=VERTEX_POINT('',#5189);
#1490=VERTEX_POINT('',#5190);
#1491=VERTEX_POINT('',#5219);
#1492=VERTEX_POINT('',#5220);
#1493=VERTEX_POINT('',#5249);
#1494=VERTEX_POINT('',#5250);
#1495=VERTEX_POINT('',#5279);
#1496=VERTEX_POINT('',#5280);
#1497=VERTEX_POINT('',#5309);
#1498=VERTEX_POINT('',#5310);
#1499=VERTEX_POINT('',#5339);
#1500=VERTEX_POINT('',#5340);
#1501=VERTEX_POINT('',#5369);
#1502=VERTEX_POINT('',#5370);
#1503=VERTEX_POINT('',#5399);
#1504=VERTEX_POINT('',#5400);
#1505=VERTEX_POINT('',#5429);
#1506=VERTEX_POINT('',#5430);
#1507=VERTEX_POINT('',#5459);
#1508=VERTEX_POINT('',#5460);
#1509=VERTEX_POINT('',#5489);
#1510=VERTEX_POINT('',#5490);
#1511=VERTEX_POINT('',#5519);
#1512=VERTEX_POINT('',#5520);
#1513=VERTEX_POINT('',#5549);
#1514=VERTEX_POINT('',#5550);
#1515=VERTEX_POINT('',#5579);
#1516=VERTEX_POINT('',#5580);
#1517=VERTEX_POINT('',#5609);
#1518=VERTEX_POINT('',#5610);
#1519=VERTEX_POINT('',#5639);
#1520=VERTEX_POINT('',#5640);
#1521=VERTEX_POINT('',#5669);
#1522=VERTEX_POINT('',#5670);
#1523=VERTEX_POINT('',#5699);
#1524=VERTEX_POINT('',#5700);
#1525=VERTEX_POINT('',#5729);
#1526=VERTEX_POINT('',#5730);
#1527=VERTEX_POINT('',#5759);
#1528=VERTEX_POINT('',#5760);
#1529=VERTEX_POINT('',#5789);
#1530=VERTEX_POINT('',#5790);
#1531=VERTEX_POINT('',#5792);
#1532=VERTEX_POINT('',#5807);
#1533=VERTEX_POINT('',#5808);
#1534=VERTEX_POINT('',#5847);
#1535=VERTEX_POINT('',#5862);
#1536=VERTEX_POINT('',#5863);
#1537=VERTEX_POINT('',#5938);
#1538=VERTEX_POINT('',#5939);
#1539=VERTEX_POINT('',#6016);
#1540=VERTEX_POINT('',#6017);
#1541=VERTEX_POINT('',#6094);
#1542=VERTEX_POINT('',#6095);
#1543=VERTEX_POINT('',#6170);
#1544=VERTEX_POINT('',#6171);
#1545=VERTEX_POINT('',#6246);
#1546=VERTEX_POINT('',#6247);
#1547=VERTEX_POINT('',#6322);
#1548=VERTEX_POINT('',#6323);
#1549=VERTEX_POINT('',#6400);
#1550=VERTEX_POINT('',#6401);
#1551=VERTEX_POINT('',#6476);
#1552=VERTEX_POINT('',#6477);
#1553=VERTEX_POINT('',#6554);
#1554=VERTEX_POINT('',#6555);
#1555=VERTEX_POINT('',#6630);
#1556=VERTEX_POINT('',#6631);
#1557=VERTEX_POINT('',#6706);
#1558=VERTEX_POINT('',#6707);
#1559=VERTEX_POINT('',#6782);
#1560=VERTEX_POINT('',#6783);
#1561=VERTEX_POINT('',#6858);
#1562=VERTEX_POINT('',#6859);
#1563=VERTEX_POINT('',#6936);
#1564=VERTEX_POINT('',#6937);
#1565=VERTEX_POINT('',#7014);
#1566=VERTEX_POINT('',#7015);
#1567=VERTEX_POINT('',#7090);
#1568=VERTEX_POINT('',#7091);
#1569=VERTEX_POINT('',#7166);
#1570=VERTEX_POINT('',#7167);
#1571=VERTEX_POINT('',#7242);
#1572=VERTEX_POINT('',#7243);
#1573=VERTEX_POINT('',#7320);
#1574=VERTEX_POINT('',#7321);
#1575=VERTEX_POINT('',#7398);
#1576=VERTEX_POINT('',#7399);
#1577=VERTEX_POINT('',#7474);
#1578=VERTEX_POINT('',#7475);
#1579=VERTEX_POINT('',#7550);
#1580=VERTEX_POINT('',#7551);
#1581=VERTEX_POINT('',#7626);
#1582=VERTEX_POINT('',#7627);
#1583=VERTEX_POINT('',#7702);
#1584=VERTEX_POINT('',#7704);
#1585=VERTEX_POINT('',#7706);
#1586=VERTEX_POINT('',#7723);
#1587=VERTEX_POINT('',#7725);
#1588=VERTEX_POINT('',#7744);
#1589=VERTEX_POINT('',#7783);
#1590=VERTEX_POINT('',#7785);
#1591=VERTEX_POINT('',#7787);
#1592=VERTEX_POINT('',#7866);
#1593=VERTEX_POINT('',#7868);
#1594=VERTEX_POINT('',#7872);
#1595=VERTEX_POINT('',#7880);
#1596=VERTEX_POINT('',#7882);
#1597=VERTEX_POINT('',#9189);
#1598=VERTEX_POINT('',#9191);
#1599=VERTEX_POINT('',#9195);
#1600=VERTEX_POINT('',#9196);
#1601=VERTEX_POINT('',#9199);
#1602=VERTEX_POINT('',#9203);
#1603=VERTEX_POINT('',#9207);
#1604=VERTEX_POINT('',#9209);
#1605=VERTEX_POINT('',#9217);
#1606=VERTEX_POINT('',#9219);
#1607=VERTEX_POINT('',#9223);
#1608=VERTEX_POINT('',#9224);
#1609=VERTEX_POINT('',#9226);
#1610=VERTEX_POINT('',#9231);
#1611=VERTEX_POINT('',#9232);
#1612=VERTEX_POINT('',#9234);
#1613=VERTEX_POINT('',#9236);
#1614=VERTEX_POINT('',#9240);
#1615=VERTEX_POINT('',#9243);
#1616=VERTEX_POINT('',#9247);
#1617=VERTEX_POINT('',#9249);
#1618=VERTEX_POINT('',#9253);
#1619=VERTEX_POINT('',#9255);
#1620=VERTEX_POINT('',#9259);
#1621=VERTEX_POINT('',#9261);
#1622=VERTEX_POINT('',#9271);
#1623=VERTEX_POINT('',#9273);
#1624=VERTEX_POINT('',#9277);
#1625=VERTEX_POINT('',#9279);
#1626=VERTEX_POINT('',#9283);
#1627=VERTEX_POINT('',#9285);
#1628=VERTEX_POINT('',#9289);
#1629=VERTEX_POINT('',#9291);
#1630=VERTEX_POINT('',#9295);
#1631=VERTEX_POINT('',#9296);
#1632=VERTEX_POINT('',#9298);
#1633=VERTEX_POINT('',#9300);
#1634=VERTEX_POINT('',#9304);
#1635=VERTEX_POINT('',#9305);
#1636=VERTEX_POINT('',#9307);
#1637=VERTEX_POINT('',#9309);
#1638=VERTEX_POINT('',#9311);
#1639=VERTEX_POINT('',#9313);
#1640=VERTEX_POINT('',#9315);
#1641=VERTEX_POINT('',#9317);
#1642=VERTEX_POINT('',#9321);
#1643=VERTEX_POINT('',#9323);
#1644=VERTEX_POINT('',#9327);
#1645=VERTEX_POINT('',#9329);
#1646=VERTEX_POINT('',#9331);
#1647=VERTEX_POINT('',#9333);
#1648=VERTEX_POINT('',#9335);
#1649=VERTEX_POINT('',#9337);
#1650=VERTEX_POINT('',#9352);
#1651=VERTEX_POINT('',#9354);
#1652=VERTEX_POINT('',#9358);
#1653=VERTEX_POINT('',#9360);
#1654=VERTEX_POINT('',#11056);
#1655=VERTEX_POINT('',#11057);
#1656=VERTEX_POINT('',#11078);
#1657=VERTEX_POINT('',#11318);
#1658=VERTEX_POINT('',#11320);
#1659=VERTEX_POINT('',#11564);
#1660=VERTEX_POINT('',#13279);
#1661=VERTEX_POINT('',#13281);
#1662=VERTEX_POINT('',#13283);
#1663=VERTEX_POINT('',#13287);
#1664=VERTEX_POINT('',#13288);
#1665=VERTEX_POINT('',#13293);
#1666=VERTEX_POINT('',#13295);
#1667=VERTEX_POINT('',#13299);
#1668=VERTEX_POINT('',#13300);
#1669=VERTEX_POINT('',#13302);
#1670=VERTEX_POINT('',#13304);
#1671=VERTEX_POINT('',#13311);
#1672=VERTEX_POINT('',#13322);
#1673=VERTEX_POINT('',#13333);
#1674=VERTEX_POINT('',#13356);
#1675=VERTEX_POINT('',#13363);
#1676=VERTEX_POINT('',#13374);
#1677=VERTEX_POINT('',#13393);
#1678=VERTEX_POINT('',#13399);
#1679=VERTEX_POINT('',#13400);
#1680=VERTEX_POINT('',#13402);
#1681=VERTEX_POINT('',#13440);
#1682=VERTEX_POINT('',#13442);
#1683=VERTEX_POINT('',#13450);
#1684=VERTEX_POINT('',#13451);
#1685=VERTEX_POINT('',#13490);
#1686=VERTEX_POINT('',#13498);
#1687=VERTEX_POINT('',#13499);
#1688=VERTEX_POINT('',#13538);
#1689=VERTEX_POINT('',#13546);
#1690=VERTEX_POINT('',#13547);
#1691=VERTEX_POINT('',#13586);
#1692=VERTEX_POINT('',#13594);
#1693=VERTEX_POINT('',#13595);
#1694=VERTEX_POINT('',#13634);
#1695=VERTEX_POINT('',#13679);
#1696=VERTEX_POINT('',#14032);
#1697=VERTEX_POINT('',#14034);
#1698=VERTEX_POINT('',#14038);
#1699=VERTEX_POINT('',#14040);
#1700=VERTEX_POINT('',#14044);
#1701=VERTEX_POINT('',#14046);
#1702=EDGE_CURVE('',#1377,#1377,#1287,.T.);
#1703=EDGE_CURVE('',#1377,#1378,#773,.T.);
#1704=EDGE_CURVE('',#1378,#1378,#1288,.T.);
#1705=EDGE_CURVE('',#1379,#1380,#1289,.T.);
#1706=EDGE_CURVE('',#1381,#1379,#774,.T.);
#1707=EDGE_CURVE('',#1381,#1382,#1290,.T.);
#1708=EDGE_CURVE('',#1380,#1382,#775,.T.);
#1709=EDGE_CURVE('',#1380,#1383,#776,.T.);
#1710=EDGE_CURVE('',#1383,#1384,#777,.T.);
#1711=EDGE_CURVE('',#1384,#1385,#778,.T.);
#1712=EDGE_CURVE('',#1385,#1386,#1291,.T.);
#1713=EDGE_CURVE('',#1386,#1387,#779,.T.);
#1714=EDGE_CURVE('',#1387,#1388,#780,.T.);
#1715=EDGE_CURVE('',#1388,#1379,#781,.T.);
#1716=EDGE_CURVE('',#1389,#1385,#782,.T.);
#1717=EDGE_CURVE('',#1389,#1390,#1292,.T.);
#1718=EDGE_CURVE('',#1386,#1390,#783,.T.);
#1719=EDGE_CURVE('',#1391,#1389,#784,.T.);
#1720=EDGE_CURVE('',#1392,#1391,#785,.T.);
#1721=EDGE_CURVE('',#1382,#1392,#786,.T.);
#1722=EDGE_CURVE('',#1393,#1381,#787,.T.);
#1723=EDGE_CURVE('',#1394,#1393,#788,.T.);
#1724=EDGE_CURVE('',#1390,#1394,#789,.T.);
#1725=EDGE_CURVE('',#1395,#1393,#790,.T.);
#1726=EDGE_CURVE('',#1396,#1395,#791,.T.);
#1727=EDGE_CURVE('',#1396,#1394,#792,.T.);
#1728=EDGE_CURVE('',#1397,#1388,#793,.T.);
#1729=EDGE_CURVE('',#1395,#1397,#794,.T.);
#1730=EDGE_CURVE('',#1398,#1387,#795,.T.);
#1731=EDGE_CURVE('',#1397,#1398,#796,.T.);
#1732=EDGE_CURVE('',#1398,#1396,#797,.T.);
#1733=EDGE_CURVE('',#1399,#1383,#798,.T.);
#1734=EDGE_CURVE('',#1400,#1399,#799,.T.);
#1735=EDGE_CURVE('',#1400,#1384,#800,.T.);
#1736=EDGE_CURVE('',#1401,#1392,#801,.T.);
#1737=EDGE_CURVE('',#1399,#1401,#802,.T.);
#1738=EDGE_CURVE('',#1402,#1391,#803,.T.);
#1739=EDGE_CURVE('',#1401,#1402,#804,.T.);
#1740=EDGE_CURVE('',#1402,#1400,#805,.T.);
#1741=EDGE_CURVE('',#1403,#1403,#1293,.T.);
#1742=EDGE_CURVE('',#1403,#1404,#806,.T.);
#1743=EDGE_CURVE('',#1404,#1404,#1294,.T.);
#1744=EDGE_CURVE('',#1405,#1405,#1295,.T.);
#1745=EDGE_CURVE('',#1405,#1406,#807,.T.);
#1746=EDGE_CURVE('',#1406,#1406,#1296,.T.);
#1747=EDGE_CURVE('',#1407,#1407,#1297,.T.);
#1748=EDGE_CURVE('',#1407,#1408,#808,.T.);
#1749=EDGE_CURVE('',#1408,#1408,#1298,.T.);
#1750=EDGE_CURVE('',#1409,#1410,#1299,.T.);
#1751=EDGE_CURVE('',#1411,#1410,#809,.T.);
#1752=EDGE_CURVE('',#1412,#1411,#1300,.T.);
#1753=EDGE_CURVE('',#1409,#1412,#810,.T.);
#1754=EDGE_CURVE('',#1413,#1414,#1301,.T.);
#1755=EDGE_CURVE('',#1415,#1414,#811,.T.);
#1756=EDGE_CURVE('',#1416,#1415,#1302,.T.);
#1757=EDGE_CURVE('',#1413,#1416,#812,.T.);
#1758=EDGE_CURVE('',#1417,#1418,#813,.T.);
#1759=EDGE_CURVE('',#1418,#1419,#814,.T.);
#1760=EDGE_CURVE('',#1420,#1419,#815,.T.);
#1761=EDGE_CURVE('',#1421,#1420,#816,.T.);
#1762=EDGE_CURVE('',#1421,#1422,#817,.T.);
#1763=EDGE_CURVE('',#1422,#1423,#818,.T.);
#1764=EDGE_CURVE('',#1424,#1423,#819,.T.);
#1765=EDGE_CURVE('',#1424,#1425,#820,.T.);
#1766=EDGE_CURVE('',#1425,#1426,#821,.T.);
#1767=EDGE_CURVE('',#1426,#1427,#822,.T.);
#1768=EDGE_CURVE('',#1428,#1427,#823,.T.);
#1769=EDGE_CURVE('',#1417,#1428,#824,.T.);
#1770=EDGE_CURVE('',#1428,#1429,#825,.T.);
#1771=EDGE_CURVE('',#1427,#1430,#826,.T.);
#1772=EDGE_CURVE('',#1429,#1430,#827,.T.);
#1773=EDGE_CURVE('',#1411,#1431,#828,.T.);
#1774=EDGE_CURVE('',#1431,#1432,#829,.T.);
#1775=EDGE_CURVE('',#1433,#1432,#830,.T.);
#1776=EDGE_CURVE('',#1433,#1434,#1303,.T.);
#1777=EDGE_CURVE('',#1435,#1434,#831,.T.);
#1778=EDGE_CURVE('',#1435,#1436,#832,.T.);
#1779=EDGE_CURVE('',#1436,#1437,#833,.T.);
#1780=EDGE_CURVE('',#1437,#1438,#834,.T.);
#1781=EDGE_CURVE('',#1438,#1439,#835,.T.);
#1782=EDGE_CURVE('',#1439,#1440,#836,.T.);
#1783=EDGE_CURVE('',#1440,#1412,#837,.T.);
#1784=EDGE_CURVE('',#1441,#1409,#838,.T.);
#1785=EDGE_CURVE('',#1440,#1441,#839,.T.);
#1786=EDGE_CURVE('',#1442,#1434,#840,.T.);
#1787=EDGE_CURVE('',#1443,#1442,#841,.T.);
#1788=EDGE_CURVE('',#1435,#1443,#842,.T.);
#1789=EDGE_CURVE('',#1444,#1445,#843,.T.);
#1790=EDGE_CURVE('',#1446,#1445,#844,.T.);
#1791=EDGE_CURVE('',#1429,#1446,#845,.T.);
#1792=EDGE_CURVE('',#1447,#1430,#846,.T.);
#1793=EDGE_CURVE('',#1448,#1447,#847,.T.);
#1794=EDGE_CURVE('',#1449,#1448,#848,.T.);
#1795=EDGE_CURVE('',#1444,#1449,#849,.T.);
#1796=EDGE_CURVE('',#1439,#1450,#850,.T.);
#1797=EDGE_CURVE('',#1450,#1451,#851,.T.);
#1798=EDGE_CURVE('',#1451,#1452,#852,.T.);
#1799=EDGE_CURVE('',#1452,#1453,#853,.T.);
#1800=EDGE_CURVE('',#1454,#1453,#854,.T.);
#1801=EDGE_CURVE('',#1454,#1455,#855,.T.);
#1802=EDGE_CURVE('',#1436,#1455,#856,.T.);
#1803=EDGE_CURVE('',#1441,#1443,#857,.T.);
#1804=EDGE_CURVE('',#1451,#1413,#858,.T.);
#1805=EDGE_CURVE('',#1452,#1416,#859,.T.);
#1806=EDGE_CURVE('',#1454,#1456,#860,.T.);
#1807=EDGE_CURVE('',#1453,#1457,#861,.T.);
#1808=EDGE_CURVE('',#1456,#1457,#862,.T.);
#1809=EDGE_CURVE('',#1415,#1425,#863,.T.);
#1810=EDGE_CURVE('',#1414,#1426,#864,.T.);
#1811=EDGE_CURVE('',#1458,#1424,#865,.T.);
#1812=EDGE_CURVE('',#1459,#1423,#866,.T.);
#1813=EDGE_CURVE('',#1458,#1459,#867,.T.);
#1814=EDGE_CURVE('',#1458,#1457,#1304,.T.);
#1815=EDGE_CURVE('',#1438,#1460,#868,.T.);
#1816=EDGE_CURVE('',#1437,#1461,#869,.T.);
#1817=EDGE_CURVE('',#1460,#1461,#870,.T.);
#1818=EDGE_CURVE('',#1460,#1450,#871,.T.);
#1819=EDGE_CURVE('',#1455,#1461,#872,.T.);
#1820=EDGE_CURVE('',#1459,#1456,#1305,.T.);
#1821=EDGE_CURVE('',#1447,#1422,#873,.T.);
#1822=EDGE_CURVE('',#1421,#1448,#874,.T.);
#1823=EDGE_CURVE('',#1462,#1463,#875,.T.);
#1824=EDGE_CURVE('',#1463,#1418,#1306,.T.);
#1825=EDGE_CURVE('',#1417,#1446,#876,.T.);
#1826=EDGE_CURVE('',#1445,#1464,#877,.T.);
#1827=EDGE_CURVE('',#1464,#1465,#878,.T.);
#1828=EDGE_CURVE('',#1466,#1465,#879,.T.);
#1829=EDGE_CURVE('',#1431,#1466,#880,.T.);
#1830=EDGE_CURVE('',#1410,#1462,#881,.T.);
#1831=EDGE_CURVE('',#1419,#1467,#1307,.T.);
#1832=EDGE_CURVE('',#1468,#1467,#882,.T.);
#1833=EDGE_CURVE('',#1469,#1468,#883,.T.);
#1834=EDGE_CURVE('',#1433,#1469,#884,.T.);
#1835=EDGE_CURVE('',#1432,#1470,#885,.T.);
#1836=EDGE_CURVE('',#1470,#1471,#886,.T.);
#1837=EDGE_CURVE('',#1472,#1471,#887,.T.);
#1838=EDGE_CURVE('',#1444,#1472,#888,.T.);
#1839=EDGE_CURVE('',#1420,#1449,#889,.T.);
#1840=EDGE_CURVE('',#1468,#1462,#890,.T.);
#1841=EDGE_CURVE('',#1469,#1442,#1308,.T.);
#1842=EDGE_CURVE('',#1464,#1472,#891,.T.);
#1843=EDGE_CURVE('',#1465,#1471,#892,.T.);
#1844=EDGE_CURVE('',#1466,#1470,#893,.T.);
#1845=EDGE_CURVE('',#1467,#1463,#894,.T.);
#1846=EDGE_CURVE('',#1473,#1474,#895,.T.);
#1847=EDGE_CURVE('',#1473,#1475,#151,.T.);
#1848=EDGE_CURVE('',#1475,#1476,#896,.T.);
#1849=EDGE_CURVE('',#1474,#1476,#152,.T.);
#1850=EDGE_CURVE('',#1477,#1478,#897,.T.);
#1851=EDGE_CURVE('',#1477,#1473,#153,.T.);
#1852=EDGE_CURVE('',#1478,#1474,#154,.T.);
#1853=EDGE_CURVE('',#1479,#1480,#898,.T.);
#1854=EDGE_CURVE('',#1479,#1477,#155,.T.);
#1855=EDGE_CURVE('',#1480,#1478,#156,.T.);
#1856=EDGE_CURVE('',#1481,#1482,#899,.T.);
#1857=EDGE_CURVE('',#1481,#1479,#157,.T.);
#1858=EDGE_CURVE('',#1482,#1480,#158,.T.);
#1859=EDGE_CURVE('',#1483,#1484,#900,.T.);
#1860=EDGE_CURVE('',#1483,#1481,#159,.T.);
#1861=EDGE_CURVE('',#1484,#1482,#160,.T.);
#1862=EDGE_CURVE('',#1485,#1486,#901,.T.);
#1863=EDGE_CURVE('',#1485,#1483,#161,.T.);
#1864=EDGE_CURVE('',#1486,#1484,#162,.T.);
#1865=EDGE_CURVE('',#1487,#1488,#902,.T.);
#1866=EDGE_CURVE('',#1487,#1485,#163,.T.);
#1867=EDGE_CURVE('',#1488,#1486,#164,.T.);
#1868=EDGE_CURVE('',#1489,#1490,#903,.T.);
#1869=EDGE_CURVE('',#1489,#1487,#165,.T.);
#1870=EDGE_CURVE('',#1490,#1488,#166,.T.);
#1871=EDGE_CURVE('',#1491,#1492,#904,.T.);
#1872=EDGE_CURVE('',#1491,#1489,#167,.T.);
#1873=EDGE_CURVE('',#1492,#1490,#168,.T.);
#1874=EDGE_CURVE('',#1493,#1494,#905,.T.);
#1875=EDGE_CURVE('',#1493,#1491,#169,.T.);
#1876=EDGE_CURVE('',#1494,#1492,#170,.T.);
#1877=EDGE_CURVE('',#1495,#1496,#906,.T.);
#1878=EDGE_CURVE('',#1495,#1493,#171,.T.);
#1879=EDGE_CURVE('',#1496,#1494,#172,.T.);
#1880=EDGE_CURVE('',#1497,#1498,#907,.T.);
#1881=EDGE_CURVE('',#1497,#1495,#173,.T.);
#1882=EDGE_CURVE('',#1498,#1496,#174,.T.);
#1883=EDGE_CURVE('',#1499,#1500,#908,.T.);
#1884=EDGE_CURVE('',#1499,#1497,#175,.T.);
#1885=EDGE_CURVE('',#1500,#1498,#176,.T.);
#1886=EDGE_CURVE('',#1501,#1502,#909,.T.);
#1887=EDGE_CURVE('',#1501,#1499,#177,.T.);
#1888=EDGE_CURVE('',#1502,#1500,#178,.T.);
#1889=EDGE_CURVE('',#1503,#1504,#910,.T.);
#1890=EDGE_CURVE('',#1503,#1501,#179,.T.);
#1891=EDGE_CURVE('',#1504,#1502,#180,.T.);
#1892=EDGE_CURVE('',#1505,#1506,#911,.T.);
#1893=EDGE_CURVE('',#1505,#1503,#181,.T.);
#1894=EDGE_CURVE('',#1506,#1504,#182,.T.);
#1895=EDGE_CURVE('',#1507,#1508,#912,.T.);
#1896=EDGE_CURVE('',#1507,#1505,#183,.T.);
#1897=EDGE_CURVE('',#1508,#1506,#184,.T.);
#1898=EDGE_CURVE('',#1509,#1510,#913,.T.);
#1899=EDGE_CURVE('',#1509,#1507,#185,.T.);
#1900=EDGE_CURVE('',#1510,#1508,#186,.T.);
#1901=EDGE_CURVE('',#1511,#1512,#914,.T.);
#1902=EDGE_CURVE('',#1511,#1509,#187,.T.);
#1903=EDGE_CURVE('',#1512,#1510,#188,.T.);
#1904=EDGE_CURVE('',#1513,#1514,#915,.T.);
#1905=EDGE_CURVE('',#1513,#1511,#189,.T.);
#1906=EDGE_CURVE('',#1514,#1512,#190,.T.);
#1907=EDGE_CURVE('',#1515,#1516,#916,.T.);
#1908=EDGE_CURVE('',#1515,#1513,#191,.T.);
#1909=EDGE_CURVE('',#1516,#1514,#192,.T.);
#1910=EDGE_CURVE('',#1517,#1518,#917,.T.);
#1911=EDGE_CURVE('',#1517,#1515,#193,.T.);
#1912=EDGE_CURVE('',#1518,#1516,#194,.T.);
#1913=EDGE_CURVE('',#1519,#1520,#918,.T.);
#1914=EDGE_CURVE('',#1519,#1517,#195,.T.);
#1915=EDGE_CURVE('',#1520,#1518,#196,.T.);
#1916=EDGE_CURVE('',#1521,#1522,#919,.T.);
#1917=EDGE_CURVE('',#1521,#1519,#197,.T.);
#1918=EDGE_CURVE('',#1522,#1520,#198,.T.);
#1919=EDGE_CURVE('',#1523,#1524,#920,.T.);
#1920=EDGE_CURVE('',#1523,#1521,#199,.T.);
#1921=EDGE_CURVE('',#1524,#1522,#200,.T.);
#1922=EDGE_CURVE('',#1525,#1526,#921,.T.);
#1923=EDGE_CURVE('',#1525,#1523,#201,.T.);
#1924=EDGE_CURVE('',#1526,#1524,#202,.T.);
#1925=EDGE_CURVE('',#1527,#1528,#922,.T.);
#1926=EDGE_CURVE('',#1527,#1525,#203,.T.);
#1927=EDGE_CURVE('',#1528,#1526,#204,.T.);
#1928=EDGE_CURVE('',#1529,#1530,#923,.T.);
#1929=EDGE_CURVE('',#1531,#1529,#73,.F.);
#1930=EDGE_CURVE('',#1530,#1531,#1309,.T.);
#1931=EDGE_CURVE('',#1532,#1533,#924,.T.);
#1932=EDGE_CURVE('',#1529,#1532,#74,.F.);
#1933=EDGE_CURVE('',#1531,#1530,#1310,.T.);
#1934=EDGE_CURVE('',#1531,#1534,#925,.T.);
#1935=EDGE_CURVE('',#1534,#1533,#75,.T.);
#1936=EDGE_CURVE('',#1535,#1536,#926,.T.);
#1937=EDGE_CURVE('',#1532,#1535,#76,.F.);
#1938=EDGE_CURVE('',#1533,#1536,#77,.T.);
#1939=EDGE_CURVE('',#1537,#1538,#927,.T.);
#1940=EDGE_CURVE('',#1535,#1537,#78,.F.);
#1941=EDGE_CURVE('',#1536,#1538,#79,.T.);
#1942=EDGE_CURVE('',#1539,#1540,#928,.T.);
#1943=EDGE_CURVE('',#1537,#1539,#80,.F.);
#1944=EDGE_CURVE('',#1538,#1540,#81,.T.);
#1945=EDGE_CURVE('',#1541,#1542,#929,.T.);
#1946=EDGE_CURVE('',#1539,#1541,#82,.F.);
#1947=EDGE_CURVE('',#1540,#1542,#83,.T.);
#1948=EDGE_CURVE('',#1543,#1544,#930,.T.);
#1949=EDGE_CURVE('',#1541,#1543,#84,.F.);
#1950=EDGE_CURVE('',#1542,#1544,#85,.T.);
#1951=EDGE_CURVE('',#1545,#1546,#931,.T.);
#1952=EDGE_CURVE('',#1543,#1545,#86,.F.);
#1953=EDGE_CURVE('',#1544,#1546,#87,.T.);
#1954=EDGE_CURVE('',#1547,#1548,#932,.T.);
#1955=EDGE_CURVE('',#1545,#1547,#88,.F.);
#1956=EDGE_CURVE('',#1546,#1548,#89,.T.);
#1957=EDGE_CURVE('',#1549,#1550,#933,.T.);
#1958=EDGE_CURVE('',#1547,#1549,#90,.F.);
#1959=EDGE_CURVE('',#1548,#1550,#91,.T.);
#1960=EDGE_CURVE('',#1551,#1552,#934,.T.);
#1961=EDGE_CURVE('',#1549,#1551,#92,.F.);
#1962=EDGE_CURVE('',#1550,#1552,#93,.T.);
#1963=EDGE_CURVE('',#1553,#1554,#935,.T.);
#1964=EDGE_CURVE('',#1551,#1553,#94,.F.);
#1965=EDGE_CURVE('',#1552,#1554,#95,.T.);
#1966=EDGE_CURVE('',#1555,#1556,#936,.T.);
#1967=EDGE_CURVE('',#1553,#1555,#96,.F.);
#1968=EDGE_CURVE('',#1554,#1556,#97,.T.);
#1969=EDGE_CURVE('',#1557,#1558,#937,.T.);
#1970=EDGE_CURVE('',#1555,#1557,#98,.F.);
#1971=EDGE_CURVE('',#1556,#1558,#99,.T.);
#1972=EDGE_CURVE('',#1559,#1560,#938,.T.);
#1973=EDGE_CURVE('',#1557,#1559,#100,.F.);
#1974=EDGE_CURVE('',#1558,#1560,#101,.T.);
#1975=EDGE_CURVE('',#1561,#1562,#939,.T.);
#1976=EDGE_CURVE('',#1559,#1561,#102,.F.);
#1977=EDGE_CURVE('',#1560,#1562,#103,.T.);
#1978=EDGE_CURVE('',#1563,#1564,#940,.T.);
#1979=EDGE_CURVE('',#1561,#1563,#104,.F.);
#1980=EDGE_CURVE('',#1562,#1564,#105,.T.);
#1981=EDGE_CURVE('',#1565,#1566,#941,.T.);
#1982=EDGE_CURVE('',#1563,#1565,#106,.F.);
#1983=EDGE_CURVE('',#1564,#1566,#107,.T.);
#1984=EDGE_CURVE('',#1567,#1568,#942,.T.);
#1985=EDGE_CURVE('',#1565,#1567,#108,.F.);
#1986=EDGE_CURVE('',#1566,#1568,#109,.T.);
#1987=EDGE_CURVE('',#1569,#1570,#943,.T.);
#1988=EDGE_CURVE('',#1567,#1569,#110,.F.);
#1989=EDGE_CURVE('',#1568,#1570,#111,.T.);
#1990=EDGE_CURVE('',#1571,#1572,#944,.T.);
#1991=EDGE_CURVE('',#1569,#1571,#112,.F.);
#1992=EDGE_CURVE('',#1570,#1572,#113,.T.);
#1993=EDGE_CURVE('',#1573,#1574,#945,.T.);
#1994=EDGE_CURVE('',#1571,#1573,#114,.F.);
#1995=EDGE_CURVE('',#1572,#1574,#115,.T.);
#1996=EDGE_CURVE('',#1575,#1576,#946,.T.);
#1997=EDGE_CURVE('',#1573,#1575,#116,.F.);
#1998=EDGE_CURVE('',#1574,#1576,#117,.T.);
#1999=EDGE_CURVE('',#1577,#1578,#947,.T.);
#2000=EDGE_CURVE('',#1575,#1577,#118,.F.);
#2001=EDGE_CURVE('',#1576,#1578,#119,.T.);
#2002=EDGE_CURVE('',#1579,#1580,#948,.T.);
#2003=EDGE_CURVE('',#1577,#1579,#120,.F.);
#2004=EDGE_CURVE('',#1578,#1580,#121,.T.);
#2005=EDGE_CURVE('',#1581,#1582,#949,.T.);
#2006=EDGE_CURVE('',#1579,#1581,#122,.F.);
#2007=EDGE_CURVE('',#1580,#1582,#123,.T.);
#2008=EDGE_CURVE('',#1583,#1583,#1311,.T.);
#2009=EDGE_CURVE('',#1583,#1584,#950,.T.);
#2010=EDGE_CURVE('',#1584,#1585,#124,.T.);
#2011=EDGE_CURVE('',#1585,#1586,#951,.T.);
#2012=EDGE_CURVE('',#1587,#1586,#125,.F.);
#2013=EDGE_CURVE('',#1587,#1588,#952,.T.);
#2014=EDGE_CURVE('',#1588,#1584,#126,.T.);
#2015=EDGE_CURVE('',#1589,#1589,#1312,.T.);
#2016=EDGE_CURVE('',#1589,#1590,#1313,.T.);
#2017=EDGE_CURVE('',#1591,#1590,#1314,.T.);
#2018=EDGE_CURVE('',#1590,#1591,#1315,.T.);
#2019=EDGE_CURVE('',#1581,#1587,#127,.F.);
#2020=EDGE_CURVE('',#1582,#1588,#128,.T.);
#2021=EDGE_CURVE('',#1592,#1592,#1316,.T.);
#2022=EDGE_CURVE('',#1592,#1593,#953,.T.);
#2023=EDGE_CURVE('',#1593,#1593,#1317,.T.);
#2024=EDGE_CURVE('',#1591,#1594,#954,.T.);
#2025=EDGE_CURVE('',#1594,#1594,#1318,.T.);
#2026=EDGE_CURVE('',#1595,#1531,#955,.T.);
#2027=EDGE_CURVE('',#1596,#1595,#956,.T.);
#2028=EDGE_CURVE('',#1534,#1596,#957,.T.);
#2029=EDGE_CURVE('',#1586,#1475,#958,.T.);
#2030=EDGE_CURVE('',#1476,#1585,#959,.T.);
#2031=EDGE_CURVE('',#1595,#1527,#205,.T.);
#2032=EDGE_CURVE('',#1596,#1528,#206,.T.);
#2033=EDGE_CURVE('',#1597,#1597,#1319,.T.);
#2034=EDGE_CURVE('',#1597,#1598,#960,.T.);
#2035=EDGE_CURVE('',#1598,#1598,#1320,.T.);
#2036=EDGE_CURVE('',#1599,#1600,#1321,.T.);
#2037=EDGE_CURVE('',#1600,#1599,#1322,.T.);
#2038=EDGE_CURVE('',#1600,#1601,#961,.T.);
#2039=EDGE_CURVE('',#1601,#1601,#1323,.T.);
#2040=EDGE_CURVE('',#1599,#1602,#962,.T.);
#2041=EDGE_CURVE('',#1602,#1602,#1324,.T.);
#2042=EDGE_CURVE('',#1603,#1603,#1325,.T.);
#2043=EDGE_CURVE('',#1603,#1604,#963,.T.);
#2044=EDGE_CURVE('',#1604,#1604,#1326,.T.);
#2045=EDGE_CURVE('',#1605,#1605,#1327,.T.);
#2046=EDGE_CURVE('',#1605,#1606,#964,.T.);
#2047=EDGE_CURVE('',#1606,#1606,#1328,.T.);
#2048=EDGE_CURVE('',#1607,#1608,#1329,.T.);
#2049=EDGE_CURVE('',#1608,#1609,#965,.T.);
#2050=EDGE_CURVE('',#1609,#1609,#1330,.T.);
#2051=EDGE_CURVE('',#1608,#1607,#1331,.T.);
#2052=EDGE_CURVE('',#1610,#1611,#1332,.T.);
#2053=EDGE_CURVE('',#1610,#1612,#966,.T.);
#2054=EDGE_CURVE('',#1612,#1613,#1333,.T.);
#2055=EDGE_CURVE('',#1611,#1613,#967,.T.);
#2056=EDGE_CURVE('',#1611,#1614,#968,.T.);
#2057=EDGE_CURVE('',#1607,#1614,#969,.T.);
#2058=EDGE_CURVE('',#1615,#1607,#970,.T.);
#2059=EDGE_CURVE('',#1610,#1615,#971,.T.);
#2060=EDGE_CURVE('',#1612,#1616,#972,.T.);
#2061=EDGE_CURVE('',#1616,#1617,#973,.T.);
#2062=EDGE_CURVE('',#1613,#1617,#974,.T.);
#2063=EDGE_CURVE('',#1617,#1618,#1334,.T.);
#2064=EDGE_CURVE('',#1619,#1618,#975,.T.);
#2065=EDGE_CURVE('',#1619,#1614,#1335,.T.);
#2066=EDGE_CURVE('',#1620,#1616,#1336,.T.);
#2067=EDGE_CURVE('',#1615,#1621,#1337,.T.);
#2068=EDGE_CURVE('',#1621,#1620,#976,.T.);
#2069=EDGE_CURVE('',#1618,#1620,#977,.T.);
#2070=EDGE_CURVE('',#1621,#1619,#978,.T.);
#2071=EDGE_CURVE('',#1622,#1622,#1338,.T.);
#2072=EDGE_CURVE('',#1622,#1623,#979,.T.);
#2073=EDGE_CURVE('',#1623,#1623,#1339,.T.);
#2074=EDGE_CURVE('',#1624,#1624,#1340,.T.);
#2075=EDGE_CURVE('',#1624,#1625,#980,.T.);
#2076=EDGE_CURVE('',#1625,#1625,#1341,.T.);
#2077=EDGE_CURVE('',#1626,#1626,#1342,.T.);
#2078=EDGE_CURVE('',#1626,#1627,#981,.T.);
#2079=EDGE_CURVE('',#1627,#1627,#1343,.T.);
#2080=EDGE_CURVE('',#1628,#1628,#1344,.T.);
#2081=EDGE_CURVE('',#1628,#1629,#982,.T.);
#2082=EDGE_CURVE('',#1629,#1629,#1345,.T.);
#2083=EDGE_CURVE('',#1630,#1631,#1346,.T.);
#2084=EDGE_CURVE('',#1632,#1630,#983,.T.);
#2085=EDGE_CURVE('',#1633,#1632,#1347,.T.);
#2086=EDGE_CURVE('',#1631,#1633,#984,.T.);
#2087=EDGE_CURVE('',#1634,#1635,#985,.T.);
#2088=EDGE_CURVE('',#1636,#1635,#986,.T.);
#2089=EDGE_CURVE('',#1637,#1636,#987,.T.);
#2090=EDGE_CURVE('',#1638,#1637,#988,.T.);
#2091=EDGE_CURVE('',#1638,#1639,#989,.T.);
#2092=EDGE_CURVE('',#1640,#1639,#990,.T.);
#2093=EDGE_CURVE('',#1641,#1640,#991,.T.);
#2094=EDGE_CURVE('',#1641,#1634,#992,.T.);
#2095=EDGE_CURVE('',#1642,#1639,#993,.T.);
#2096=EDGE_CURVE('',#1643,#1642,#994,.T.);
#2097=EDGE_CURVE('',#1643,#1640,#995,.T.);
#2098=EDGE_CURVE('',#1644,#1643,#996,.T.);
#2099=EDGE_CURVE('',#1645,#1642,#997,.T.);
#2100=EDGE_CURVE('',#1645,#1646,#998,.T.);
#2101=EDGE_CURVE('',#1646,#1647,#999,.T.);
#2102=EDGE_CURVE('',#1647,#1648,#1000,.T.);
#2103=EDGE_CURVE('',#1649,#1648,#1001,.T.);
#2104=EDGE_CURVE('',#1644,#1649,#1002,.T.);
#2105=EDGE_CURVE('',#1632,#1649,#1003,.T.);
#2106=EDGE_CURVE('',#1630,#1644,#1004,.T.);
#2107=EDGE_CURVE('',#1631,#1641,#1005,.T.);
#2108=EDGE_CURVE('',#1633,#1634,#1006,.T.);
#2109=EDGE_CURVE('',#1635,#1648,#1007,.T.);
#2110=EDGE_CURVE('',#1636,#1647,#1008,.T.);
#2111=EDGE_CURVE('',#1650,#1646,#1009,.T.);
#2112=EDGE_CURVE('',#1651,#1645,#1010,.T.);
#2113=EDGE_CURVE('',#1650,#1651,#1011,.T.);
#2114=EDGE_CURVE('',#1652,#1638,#1012,.T.);
#2115=EDGE_CURVE('',#1653,#1637,#1013,.T.);
#2116=EDGE_CURVE('',#1652,#1653,#1014,.T.);
#2117=EDGE_CURVE('',#1651,#1652,#1348,.T.);
#2118=EDGE_CURVE('',#1653,#1650,#1349,.T.);
#2119=EDGE_CURVE('',#1654,#1655,#129,.T.);
#2120=EDGE_CURVE('',#1655,#1656,#207,.T.);
#2121=EDGE_CURVE('',#1656,#1657,#1350,.T.);
#2122=EDGE_CURVE('',#1658,#1657,#208,.T.);
#2123=EDGE_CURVE('',#1658,#1654,#1351,.T.);
#2124=EDGE_CURVE('',#1659,#1658,#1352,.T.);
#2125=EDGE_CURVE('',#1659,#1654,#1015,.T.);
#2126=EDGE_CURVE('',#1655,#1659,#130,.T.);
#2127=EDGE_CURVE('',#1657,#1656,#1353,.T.);
#2128=EDGE_CURVE('',#1660,#1660,#1354,.T.);
#2129=EDGE_CURVE('',#1660,#1661,#1016,.T.);
#2130=EDGE_CURVE('',#1661,#1662,#1355,.T.);
#2131=EDGE_CURVE('',#1662,#1661,#1356,.T.);
#2132=EDGE_CURVE('',#1663,#1664,#1357,.T.);
#2133=EDGE_CURVE('',#1664,#1662,#1017,.T.);
#2134=EDGE_CURVE('',#1664,#1663,#1358,.T.);
#2135=EDGE_CURVE('',#1665,#1665,#1359,.T.);
#2136=EDGE_CURVE('',#1665,#1666,#1018,.T.);
#2137=EDGE_CURVE('',#1666,#1666,#1360,.T.);
#2138=EDGE_CURVE('',#1667,#1668,#1361,.T.);
#2139=EDGE_CURVE('',#1668,#1669,#1019,.T.);
#2140=EDGE_CURVE('',#1669,#1670,#131,.T.);
#2141=EDGE_CURVE('',#1670,#1671,#132,.T.);
#2142=EDGE_CURVE('',#1671,#1672,#133,.T.);
#2143=EDGE_CURVE('',#1672,#1673,#134,.T.);
#2144=EDGE_CURVE('',#1673,#1674,#135,.T.);
#2145=EDGE_CURVE('',#1674,#1675,#136,.T.);
#2146=EDGE_CURVE('',#1675,#1676,#137,.T.);
#2147=EDGE_CURVE('',#1676,#1669,#138,.T.);
#2148=EDGE_CURVE('',#1668,#1667,#1362,.T.);
#2149=EDGE_CURVE('',#1667,#1677,#1363,.T.);
#2150=EDGE_CURVE('',#1677,#1677,#1364,.T.);
#2151=EDGE_CURVE('',#1663,#1665,#1020,.T.);
#2152=EDGE_CURVE('',#1678,#1679,#1021,.T.);
#2153=EDGE_CURVE('',#1678,#1680,#139,.T.);
#2154=EDGE_CURVE('',#1680,#1681,#1022,.T.);
#2155=EDGE_CURVE('',#1681,#1682,#209,.T.);
#2156=EDGE_CURVE('',#1682,#1679,#210,.T.);
#2157=EDGE_CURVE('',#1683,#1684,#1023,.T.);
#2158=EDGE_CURVE('',#1683,#1678,#140,.T.);
#2159=EDGE_CURVE('',#1679,#1685,#211,.T.);
#2160=EDGE_CURVE('',#1685,#1684,#212,.T.);
#2161=EDGE_CURVE('',#1686,#1687,#1024,.T.);
#2162=EDGE_CURVE('',#1686,#1683,#141,.T.);
#2163=EDGE_CURVE('',#1688,#1684,#213,.T.);
#2164=EDGE_CURVE('',#1687,#1688,#214,.T.);
#2165=EDGE_CURVE('',#1689,#1690,#1025,.T.);
#2166=EDGE_CURVE('',#1689,#1686,#142,.T.);
#2167=EDGE_CURVE('',#1687,#1691,#215,.T.);
#2168=EDGE_CURVE('',#1691,#1690,#216,.T.);
#2169=EDGE_CURVE('',#1692,#1693,#1026,.T.);
#2170=EDGE_CURVE('',#1692,#1689,#143,.T.);
#2171=EDGE_CURVE('',#1690,#1694,#217,.T.);
#2172=EDGE_CURVE('',#1694,#1693,#218,.T.);
#2173=EDGE_CURVE('',#1680,#1692,#144,.T.);
#2174=EDGE_CURVE('',#1693,#1695,#219,.T.);
#2175=EDGE_CURVE('',#1695,#1681,#220,.T.);
#2176=EDGE_CURVE('',#1691,#1688,#1365,.T.);
#2177=EDGE_CURVE('',#1688,#1685,#1366,.T.);
#2178=EDGE_CURVE('',#1685,#1682,#1367,.T.);
#2179=EDGE_CURVE('',#1682,#1695,#1368,.T.);
#2180=EDGE_CURVE('',#1695,#1694,#1369,.T.);
#2181=EDGE_CURVE('',#1694,#1691,#1370,.T.);
#2182=EDGE_CURVE('',#1672,#1692,#145,.T.);
#2183=EDGE_CURVE('',#1689,#1671,#146,.T.);
#2184=EDGE_CURVE('',#1686,#1670,#147,.T.);
#2185=EDGE_CURVE('',#1674,#1680,#148,.T.);
#2186=EDGE_CURVE('',#1683,#1676,#149,.T.);
#2187=EDGE_CURVE('',#1675,#1678,#150,.T.);
#2188=EDGE_CURVE('',#1696,#1696,#1371,.T.);
#2189=EDGE_CURVE('',#1696,#1697,#1027,.T.);
#2190=EDGE_CURVE('',#1697,#1697,#1372,.T.);
#2191=EDGE_CURVE('',#1698,#1698,#1373,.T.);
#2192=EDGE_CURVE('',#1698,#1699,#1028,.T.);
#2193=EDGE_CURVE('',#1699,#1699,#1374,.T.);
#2194=EDGE_CURVE('',#1700,#1700,#1375,.T.);
#2195=EDGE_CURVE('',#1700,#1701,#1029,.T.);
#2196=EDGE_CURVE('',#1701,#1701,#1376,.T.);
#2197=ORIENTED_EDGE('',*,*,#1702,.T.);
#2198=ORIENTED_EDGE('',*,*,#1703,.T.);
#2199=ORIENTED_EDGE('',*,*,#1704,.F.);
#2200=ORIENTED_EDGE('',*,*,#1703,.F.);
#2201=ORIENTED_EDGE('',*,*,#1705,.F.);
#2202=ORIENTED_EDGE('',*,*,#1706,.F.);
#2203=ORIENTED_EDGE('',*,*,#1707,.T.);
#2204=ORIENTED_EDGE('',*,*,#1708,.F.);
#2205=ORIENTED_EDGE('',*,*,#1705,.T.);
#2206=ORIENTED_EDGE('',*,*,#1709,.T.);
#2207=ORIENTED_EDGE('',*,*,#1710,.T.);
#2208=ORIENTED_EDGE('',*,*,#1711,.T.);
#2209=ORIENTED_EDGE('',*,*,#1712,.T.);
#2210=ORIENTED_EDGE('',*,*,#1713,.T.);
#2211=ORIENTED_EDGE('',*,*,#1714,.T.);
#2212=ORIENTED_EDGE('',*,*,#1715,.T.);
#2213=ORIENTED_EDGE('',*,*,#1702,.F.);
#2214=ORIENTED_EDGE('',*,*,#1716,.F.);
#2215=ORIENTED_EDGE('',*,*,#1717,.T.);
#2216=ORIENTED_EDGE('',*,*,#1718,.F.);
#2217=ORIENTED_EDGE('',*,*,#1712,.F.);
#2218=ORIENTED_EDGE('',*,*,#1717,.F.);
#2219=ORIENTED_EDGE('',*,*,#1719,.F.);
#2220=ORIENTED_EDGE('',*,*,#1720,.F.);
#2221=ORIENTED_EDGE('',*,*,#1721,.F.);
#2222=ORIENTED_EDGE('',*,*,#1707,.F.);
#2223=ORIENTED_EDGE('',*,*,#1722,.F.);
#2224=ORIENTED_EDGE('',*,*,#1723,.F.);
#2225=ORIENTED_EDGE('',*,*,#1724,.F.);
#2226=ORIENTED_EDGE('',*,*,#1704,.T.);
#2227=ORIENTED_EDGE('',*,*,#1723,.T.);
#2228=ORIENTED_EDGE('',*,*,#1725,.F.);
#2229=ORIENTED_EDGE('',*,*,#1726,.F.);
#2230=ORIENTED_EDGE('',*,*,#1727,.T.);
#2231=ORIENTED_EDGE('',*,*,#1715,.F.);
#2232=ORIENTED_EDGE('',*,*,#1728,.F.);
#2233=ORIENTED_EDGE('',*,*,#1729,.F.);
#2234=ORIENTED_EDGE('',*,*,#1725,.T.);
#2235=ORIENTED_EDGE('',*,*,#1722,.T.);
#2236=ORIENTED_EDGE('',*,*,#1706,.T.);
#2237=ORIENTED_EDGE('',*,*,#1714,.F.);
#2238=ORIENTED_EDGE('',*,*,#1730,.F.);
#2239=ORIENTED_EDGE('',*,*,#1731,.F.);
#2240=ORIENTED_EDGE('',*,*,#1728,.T.);
#2241=ORIENTED_EDGE('',*,*,#1713,.F.);
#2242=ORIENTED_EDGE('',*,*,#1718,.T.);
#2243=ORIENTED_EDGE('',*,*,#1724,.T.);
#2244=ORIENTED_EDGE('',*,*,#1727,.F.);
#2245=ORIENTED_EDGE('',*,*,#1732,.F.);
#2246=ORIENTED_EDGE('',*,*,#1730,.T.);
#2247=ORIENTED_EDGE('',*,*,#1726,.T.);
#2248=ORIENTED_EDGE('',*,*,#1729,.T.);
#2249=ORIENTED_EDGE('',*,*,#1731,.T.);
#2250=ORIENTED_EDGE('',*,*,#1732,.T.);
#2251=ORIENTED_EDGE('',*,*,#1710,.F.);
#2252=ORIENTED_EDGE('',*,*,#1733,.F.);
#2253=ORIENTED_EDGE('',*,*,#1734,.F.);
#2254=ORIENTED_EDGE('',*,*,#1735,.T.);
#2255=ORIENTED_EDGE('',*,*,#1709,.F.);
#2256=ORIENTED_EDGE('',*,*,#1708,.T.);
#2257=ORIENTED_EDGE('',*,*,#1721,.T.);
#2258=ORIENTED_EDGE('',*,*,#1736,.F.);
#2259=ORIENTED_EDGE('',*,*,#1737,.F.);
#2260=ORIENTED_EDGE('',*,*,#1733,.T.);
#2261=ORIENTED_EDGE('',*,*,#1720,.T.);
#2262=ORIENTED_EDGE('',*,*,#1738,.F.);
#2263=ORIENTED_EDGE('',*,*,#1739,.F.);
#2264=ORIENTED_EDGE('',*,*,#1736,.T.);
#2265=ORIENTED_EDGE('',*,*,#1711,.F.);
#2266=ORIENTED_EDGE('',*,*,#1735,.F.);
#2267=ORIENTED_EDGE('',*,*,#1740,.F.);
#2268=ORIENTED_EDGE('',*,*,#1738,.T.);
#2269=ORIENTED_EDGE('',*,*,#1719,.T.);
#2270=ORIENTED_EDGE('',*,*,#1716,.T.);
#2271=ORIENTED_EDGE('',*,*,#1734,.T.);
#2272=ORIENTED_EDGE('',*,*,#1737,.T.);
#2273=ORIENTED_EDGE('',*,*,#1739,.T.);
#2274=ORIENTED_EDGE('',*,*,#1740,.T.);
#2275=ORIENTED_EDGE('',*,*,#1741,.T.);
#2276=ORIENTED_EDGE('',*,*,#1742,.T.);
#2277=ORIENTED_EDGE('',*,*,#1743,.F.);
#2278=ORIENTED_EDGE('',*,*,#1742,.F.);
#2279=ORIENTED_EDGE('',*,*,#1744,.F.);
#2280=ORIENTED_EDGE('',*,*,#1745,.T.);
#2281=ORIENTED_EDGE('',*,*,#1746,.F.);
#2282=ORIENTED_EDGE('',*,*,#1745,.F.);
#2283=ORIENTED_EDGE('',*,*,#1747,.F.);
#2284=ORIENTED_EDGE('',*,*,#1748,.T.);
#2285=ORIENTED_EDGE('',*,*,#1749,.T.);
#2286=ORIENTED_EDGE('',*,*,#1748,.F.);
#2287=ORIENTED_EDGE('',*,*,#1750,.T.);
#2288=ORIENTED_EDGE('',*,*,#1751,.F.);
#2289=ORIENTED_EDGE('',*,*,#1752,.F.);
#2290=ORIENTED_EDGE('',*,*,#1753,.F.);
#2291=ORIENTED_EDGE('',*,*,#1754,.T.);
#2292=ORIENTED_EDGE('',*,*,#1755,.F.);
#2293=ORIENTED_EDGE('',*,*,#1756,.F.);
#2294=ORIENTED_EDGE('',*,*,#1757,.F.);
#2295=ORIENTED_EDGE('',*,*,#1758,.T.);
#2296=ORIENTED_EDGE('',*,*,#1759,.T.);
#2297=ORIENTED_EDGE('',*,*,#1760,.F.);
#2298=ORIENTED_EDGE('',*,*,#1761,.F.);
#2299=ORIENTED_EDGE('',*,*,#1762,.T.);
#2300=ORIENTED_EDGE('',*,*,#1763,.T.);
#2301=ORIENTED_EDGE('',*,*,#1764,.F.);
#2302=ORIENTED_EDGE('',*,*,#1765,.T.);
#2303=ORIENTED_EDGE('',*,*,#1766,.T.);
#2304=ORIENTED_EDGE('',*,*,#1767,.T.);
#2305=ORIENTED_EDGE('',*,*,#1768,.F.);
#2306=ORIENTED_EDGE('',*,*,#1769,.F.);
#2307=ORIENTED_EDGE('',*,*,#1770,.F.);
#2308=ORIENTED_EDGE('',*,*,#1768,.T.);
#2309=ORIENTED_EDGE('',*,*,#1771,.T.);
#2310=ORIENTED_EDGE('',*,*,#1772,.F.);
#2311=ORIENTED_EDGE('',*,*,#1752,.T.);
#2312=ORIENTED_EDGE('',*,*,#1773,.T.);
#2313=ORIENTED_EDGE('',*,*,#1774,.T.);
#2314=ORIENTED_EDGE('',*,*,#1775,.F.);
#2315=ORIENTED_EDGE('',*,*,#1776,.T.);
#2316=ORIENTED_EDGE('',*,*,#1777,.F.);
#2317=ORIENTED_EDGE('',*,*,#1778,.T.);
#2318=ORIENTED_EDGE('',*,*,#1779,.T.);
#2319=ORIENTED_EDGE('',*,*,#1780,.T.);
#2320=ORIENTED_EDGE('',*,*,#1781,.T.);
#2321=ORIENTED_EDGE('',*,*,#1782,.T.);
#2322=ORIENTED_EDGE('',*,*,#1783,.T.);
#2323=ORIENTED_EDGE('',*,*,#1749,.F.);
#2324=ORIENTED_EDGE('',*,*,#1784,.T.);
#2325=ORIENTED_EDGE('',*,*,#1753,.T.);
#2326=ORIENTED_EDGE('',*,*,#1783,.F.);
#2327=ORIENTED_EDGE('',*,*,#1785,.T.);
#2328=ORIENTED_EDGE('',*,*,#1786,.F.);
#2329=ORIENTED_EDGE('',*,*,#1787,.F.);
#2330=ORIENTED_EDGE('',*,*,#1788,.F.);
#2331=ORIENTED_EDGE('',*,*,#1777,.T.);
#2332=ORIENTED_EDGE('',*,*,#1789,.T.);
#2333=ORIENTED_EDGE('',*,*,#1790,.F.);
#2334=ORIENTED_EDGE('',*,*,#1791,.F.);
#2335=ORIENTED_EDGE('',*,*,#1772,.T.);
#2336=ORIENTED_EDGE('',*,*,#1792,.F.);
#2337=ORIENTED_EDGE('',*,*,#1793,.F.);
#2338=ORIENTED_EDGE('',*,*,#1794,.F.);
#2339=ORIENTED_EDGE('',*,*,#1795,.F.);
#2340=ORIENTED_EDGE('',*,*,#1785,.F.);
#2341=ORIENTED_EDGE('',*,*,#1782,.F.);
#2342=ORIENTED_EDGE('',*,*,#1796,.T.);
#2343=ORIENTED_EDGE('',*,*,#1797,.T.);
#2344=ORIENTED_EDGE('',*,*,#1798,.T.);
#2345=ORIENTED_EDGE('',*,*,#1799,.T.);
#2346=ORIENTED_EDGE('',*,*,#1800,.F.);
#2347=ORIENTED_EDGE('',*,*,#1801,.T.);
#2348=ORIENTED_EDGE('',*,*,#1802,.F.);
#2349=ORIENTED_EDGE('',*,*,#1778,.F.);
#2350=ORIENTED_EDGE('',*,*,#1788,.T.);
#2351=ORIENTED_EDGE('',*,*,#1803,.F.);
#2352=ORIENTED_EDGE('',*,*,#1798,.F.);
#2353=ORIENTED_EDGE('',*,*,#1804,.T.);
#2354=ORIENTED_EDGE('',*,*,#1757,.T.);
#2355=ORIENTED_EDGE('',*,*,#1805,.F.);
#2356=ORIENTED_EDGE('',*,*,#1806,.F.);
#2357=ORIENTED_EDGE('',*,*,#1800,.T.);
#2358=ORIENTED_EDGE('',*,*,#1807,.T.);
#2359=ORIENTED_EDGE('',*,*,#1808,.F.);
#2360=ORIENTED_EDGE('',*,*,#1766,.F.);
#2361=ORIENTED_EDGE('',*,*,#1809,.F.);
#2362=ORIENTED_EDGE('',*,*,#1755,.T.);
#2363=ORIENTED_EDGE('',*,*,#1810,.T.);
#2364=ORIENTED_EDGE('',*,*,#1811,.T.);
#2365=ORIENTED_EDGE('',*,*,#1764,.T.);
#2366=ORIENTED_EDGE('',*,*,#1812,.F.);
#2367=ORIENTED_EDGE('',*,*,#1813,.F.);
#2368=ORIENTED_EDGE('',*,*,#1799,.F.);
#2369=ORIENTED_EDGE('',*,*,#1805,.T.);
#2370=ORIENTED_EDGE('',*,*,#1756,.T.);
#2371=ORIENTED_EDGE('',*,*,#1809,.T.);
#2372=ORIENTED_EDGE('',*,*,#1765,.F.);
#2373=ORIENTED_EDGE('',*,*,#1811,.F.);
#2374=ORIENTED_EDGE('',*,*,#1814,.T.);
#2375=ORIENTED_EDGE('',*,*,#1807,.F.);
#2376=ORIENTED_EDGE('',*,*,#1746,.T.);
#2377=ORIENTED_EDGE('',*,*,#1815,.F.);
#2378=ORIENTED_EDGE('',*,*,#1780,.F.);
#2379=ORIENTED_EDGE('',*,*,#1816,.T.);
#2380=ORIENTED_EDGE('',*,*,#1817,.F.);
#2381=ORIENTED_EDGE('',*,*,#1792,.T.);
#2382=ORIENTED_EDGE('',*,*,#1771,.F.);
#2383=ORIENTED_EDGE('',*,*,#1767,.F.);
#2384=ORIENTED_EDGE('',*,*,#1810,.F.);
#2385=ORIENTED_EDGE('',*,*,#1754,.F.);
#2386=ORIENTED_EDGE('',*,*,#1804,.F.);
#2387=ORIENTED_EDGE('',*,*,#1797,.F.);
#2388=ORIENTED_EDGE('',*,*,#1818,.F.);
#2389=ORIENTED_EDGE('',*,*,#1817,.T.);
#2390=ORIENTED_EDGE('',*,*,#1819,.F.);
#2391=ORIENTED_EDGE('',*,*,#1801,.F.);
#2392=ORIENTED_EDGE('',*,*,#1806,.T.);
#2393=ORIENTED_EDGE('',*,*,#1820,.F.);
#2394=ORIENTED_EDGE('',*,*,#1812,.T.);
#2395=ORIENTED_EDGE('',*,*,#1763,.F.);
#2396=ORIENTED_EDGE('',*,*,#1821,.F.);
#2397=ORIENTED_EDGE('',*,*,#1744,.T.);
#2398=ORIENTED_EDGE('',*,*,#1820,.T.);
#2399=ORIENTED_EDGE('',*,*,#1808,.T.);
#2400=ORIENTED_EDGE('',*,*,#1814,.F.);
#2401=ORIENTED_EDGE('',*,*,#1813,.T.);
#2402=ORIENTED_EDGE('',*,*,#1762,.F.);
#2403=ORIENTED_EDGE('',*,*,#1822,.T.);
#2404=ORIENTED_EDGE('',*,*,#1793,.T.);
#2405=ORIENTED_EDGE('',*,*,#1821,.T.);
#2406=ORIENTED_EDGE('',*,*,#1818,.T.);
#2407=ORIENTED_EDGE('',*,*,#1796,.F.);
#2408=ORIENTED_EDGE('',*,*,#1781,.F.);
#2409=ORIENTED_EDGE('',*,*,#1815,.T.);
#2410=ORIENTED_EDGE('',*,*,#1819,.T.);
#2411=ORIENTED_EDGE('',*,*,#1816,.F.);
#2412=ORIENTED_EDGE('',*,*,#1779,.F.);
#2413=ORIENTED_EDGE('',*,*,#1802,.T.);
#2414=ORIENTED_EDGE('',*,*,#1823,.T.);
#2415=ORIENTED_EDGE('',*,*,#1824,.T.);
#2416=ORIENTED_EDGE('',*,*,#1758,.F.);
#2417=ORIENTED_EDGE('',*,*,#1825,.T.);
#2418=ORIENTED_EDGE('',*,*,#1790,.T.);
#2419=ORIENTED_EDGE('',*,*,#1826,.T.);
#2420=ORIENTED_EDGE('',*,*,#1827,.T.);
#2421=ORIENTED_EDGE('',*,*,#1828,.F.);
#2422=ORIENTED_EDGE('',*,*,#1829,.F.);
#2423=ORIENTED_EDGE('',*,*,#1773,.F.);
#2424=ORIENTED_EDGE('',*,*,#1751,.T.);
#2425=ORIENTED_EDGE('',*,*,#1830,.T.);
#2426=ORIENTED_EDGE('',*,*,#1743,.T.);
#2427=ORIENTED_EDGE('',*,*,#1760,.T.);
#2428=ORIENTED_EDGE('',*,*,#1831,.T.);
#2429=ORIENTED_EDGE('',*,*,#1832,.F.);
#2430=ORIENTED_EDGE('',*,*,#1833,.F.);
#2431=ORIENTED_EDGE('',*,*,#1834,.F.);
#2432=ORIENTED_EDGE('',*,*,#1775,.T.);
#2433=ORIENTED_EDGE('',*,*,#1835,.T.);
#2434=ORIENTED_EDGE('',*,*,#1836,.T.);
#2435=ORIENTED_EDGE('',*,*,#1837,.F.);
#2436=ORIENTED_EDGE('',*,*,#1838,.F.);
#2437=ORIENTED_EDGE('',*,*,#1795,.T.);
#2438=ORIENTED_EDGE('',*,*,#1839,.F.);
#2439=ORIENTED_EDGE('',*,*,#1741,.F.);
#2440=ORIENTED_EDGE('',*,*,#1833,.T.);
#2441=ORIENTED_EDGE('',*,*,#1840,.T.);
#2442=ORIENTED_EDGE('',*,*,#1830,.F.);
#2443=ORIENTED_EDGE('',*,*,#1750,.F.);
#2444=ORIENTED_EDGE('',*,*,#1784,.F.);
#2445=ORIENTED_EDGE('',*,*,#1803,.T.);
#2446=ORIENTED_EDGE('',*,*,#1787,.T.);
#2447=ORIENTED_EDGE('',*,*,#1841,.F.);
#2448=ORIENTED_EDGE('',*,*,#1747,.T.);
#2449=ORIENTED_EDGE('',*,*,#1789,.F.);
#2450=ORIENTED_EDGE('',*,*,#1838,.T.);
#2451=ORIENTED_EDGE('',*,*,#1842,.F.);
#2452=ORIENTED_EDGE('',*,*,#1826,.F.);
#2453=ORIENTED_EDGE('',*,*,#1837,.T.);
#2454=ORIENTED_EDGE('',*,*,#1843,.F.);
#2455=ORIENTED_EDGE('',*,*,#1827,.F.);
#2456=ORIENTED_EDGE('',*,*,#1842,.T.);
#2457=ORIENTED_EDGE('',*,*,#1836,.F.);
#2458=ORIENTED_EDGE('',*,*,#1844,.F.);
#2459=ORIENTED_EDGE('',*,*,#1828,.T.);
#2460=ORIENTED_EDGE('',*,*,#1843,.T.);
#2461=ORIENTED_EDGE('',*,*,#1835,.F.);
#2462=ORIENTED_EDGE('',*,*,#1774,.F.);
#2463=ORIENTED_EDGE('',*,*,#1829,.T.);
#2464=ORIENTED_EDGE('',*,*,#1844,.T.);
#2465=ORIENTED_EDGE('',*,*,#1841,.T.);
#2466=ORIENTED_EDGE('',*,*,#1786,.T.);
#2467=ORIENTED_EDGE('',*,*,#1776,.F.);
#2468=ORIENTED_EDGE('',*,*,#1834,.T.);
#2469=ORIENTED_EDGE('',*,*,#1761,.T.);
#2470=ORIENTED_EDGE('',*,*,#1839,.T.);
#2471=ORIENTED_EDGE('',*,*,#1794,.T.);
#2472=ORIENTED_EDGE('',*,*,#1822,.F.);
#2473=ORIENTED_EDGE('',*,*,#1769,.T.);
#2474=ORIENTED_EDGE('',*,*,#1770,.T.);
#2475=ORIENTED_EDGE('',*,*,#1791,.T.);
#2476=ORIENTED_EDGE('',*,*,#1825,.F.);
#2477=ORIENTED_EDGE('',*,*,#1832,.T.);
#2478=ORIENTED_EDGE('',*,*,#1845,.T.);
#2479=ORIENTED_EDGE('',*,*,#1823,.F.);
#2480=ORIENTED_EDGE('',*,*,#1840,.F.);
#2481=ORIENTED_EDGE('',*,*,#1831,.F.);
#2482=ORIENTED_EDGE('',*,*,#1759,.F.);
#2483=ORIENTED_EDGE('',*,*,#1824,.F.);
#2484=ORIENTED_EDGE('',*,*,#1845,.F.);
#2485=ORIENTED_EDGE('',*,*,#1846,.F.);
#2486=ORIENTED_EDGE('',*,*,#1847,.T.);
#2487=ORIENTED_EDGE('',*,*,#1848,.T.);
#2488=ORIENTED_EDGE('',*,*,#1849,.F.);
#2489=ORIENTED_EDGE('',*,*,#1850,.F.);
#2490=ORIENTED_EDGE('',*,*,#1851,.T.);
#2491=ORIENTED_EDGE('',*,*,#1846,.T.);
#2492=ORIENTED_EDGE('',*,*,#1852,.F.);
#2493=ORIENTED_EDGE('',*,*,#1853,.F.);
#2494=ORIENTED_EDGE('',*,*,#1854,.T.);
#2495=ORIENTED_EDGE('',*,*,#1850,.T.);
#2496=ORIENTED_EDGE('',*,*,#1855,.F.);
#2497=ORIENTED_EDGE('',*,*,#1856,.F.);
#2498=ORIENTED_EDGE('',*,*,#1857,.T.);
#2499=ORIENTED_EDGE('',*,*,#1853,.T.);
#2500=ORIENTED_EDGE('',*,*,#1858,.F.);
#2501=ORIENTED_EDGE('',*,*,#1859,.F.);
#2502=ORIENTED_EDGE('',*,*,#1860,.T.);
#2503=ORIENTED_EDGE('',*,*,#1856,.T.);
#2504=ORIENTED_EDGE('',*,*,#1861,.F.);
#2505=ORIENTED_EDGE('',*,*,#1862,.F.);
#2506=ORIENTED_EDGE('',*,*,#1863,.T.);
#2507=ORIENTED_EDGE('',*,*,#1859,.T.);
#2508=ORIENTED_EDGE('',*,*,#1864,.F.);
#2509=ORIENTED_EDGE('',*,*,#1865,.F.);
#2510=ORIENTED_EDGE('',*,*,#1866,.T.);
#2511=ORIENTED_EDGE('',*,*,#1862,.T.);
#2512=ORIENTED_EDGE('',*,*,#1867,.F.);
#2513=ORIENTED_EDGE('',*,*,#1868,.F.);
#2514=ORIENTED_EDGE('',*,*,#1869,.T.);
#2515=ORIENTED_EDGE('',*,*,#1865,.T.);
#2516=ORIENTED_EDGE('',*,*,#1870,.F.);
#2517=ORIENTED_EDGE('',*,*,#1871,.F.);
#2518=ORIENTED_EDGE('',*,*,#1872,.T.);
#2519=ORIENTED_EDGE('',*,*,#1868,.T.);
#2520=ORIENTED_EDGE('',*,*,#1873,.F.);
#2521=ORIENTED_EDGE('',*,*,#1874,.F.);
#2522=ORIENTED_EDGE('',*,*,#1875,.T.);
#2523=ORIENTED_EDGE('',*,*,#1871,.T.);
#2524=ORIENTED_EDGE('',*,*,#1876,.F.);
#2525=ORIENTED_EDGE('',*,*,#1877,.F.);
#2526=ORIENTED_EDGE('',*,*,#1878,.T.);
#2527=ORIENTED_EDGE('',*,*,#1874,.T.);
#2528=ORIENTED_EDGE('',*,*,#1879,.F.);
#2529=ORIENTED_EDGE('',*,*,#1880,.F.);
#2530=ORIENTED_EDGE('',*,*,#1881,.T.);
#2531=ORIENTED_EDGE('',*,*,#1877,.T.);
#2532=ORIENTED_EDGE('',*,*,#1882,.F.);
#2533=ORIENTED_EDGE('',*,*,#1883,.F.);
#2534=ORIENTED_EDGE('',*,*,#1884,.T.);
#2535=ORIENTED_EDGE('',*,*,#1880,.T.);
#2536=ORIENTED_EDGE('',*,*,#1885,.F.);
#2537=ORIENTED_EDGE('',*,*,#1886,.F.);
#2538=ORIENTED_EDGE('',*,*,#1887,.T.);
#2539=ORIENTED_EDGE('',*,*,#1883,.T.);
#2540=ORIENTED_EDGE('',*,*,#1888,.F.);
#2541=ORIENTED_EDGE('',*,*,#1889,.F.);
#2542=ORIENTED_EDGE('',*,*,#1890,.T.);
#2543=ORIENTED_EDGE('',*,*,#1886,.T.);
#2544=ORIENTED_EDGE('',*,*,#1891,.F.);
#2545=ORIENTED_EDGE('',*,*,#1892,.F.);
#2546=ORIENTED_EDGE('',*,*,#1893,.T.);
#2547=ORIENTED_EDGE('',*,*,#1889,.T.);
#2548=ORIENTED_EDGE('',*,*,#1894,.F.);
#2549=ORIENTED_EDGE('',*,*,#1895,.F.);
#2550=ORIENTED_EDGE('',*,*,#1896,.T.);
#2551=ORIENTED_EDGE('',*,*,#1892,.T.);
#2552=ORIENTED_EDGE('',*,*,#1897,.F.);
#2553=ORIENTED_EDGE('',*,*,#1898,.F.);
#2554=ORIENTED_EDGE('',*,*,#1899,.T.);
#2555=ORIENTED_EDGE('',*,*,#1895,.T.);
#2556=ORIENTED_EDGE('',*,*,#1900,.F.);
#2557=ORIENTED_EDGE('',*,*,#1901,.F.);
#2558=ORIENTED_EDGE('',*,*,#1902,.T.);
#2559=ORIENTED_EDGE('',*,*,#1898,.T.);
#2560=ORIENTED_EDGE('',*,*,#1903,.F.);
#2561=ORIENTED_EDGE('',*,*,#1904,.F.);
#2562=ORIENTED_EDGE('',*,*,#1905,.T.);
#2563=ORIENTED_EDGE('',*,*,#1901,.T.);
#2564=ORIENTED_EDGE('',*,*,#1906,.F.);
#2565=ORIENTED_EDGE('',*,*,#1907,.F.);
#2566=ORIENTED_EDGE('',*,*,#1908,.T.);
#2567=ORIENTED_EDGE('',*,*,#1904,.T.);
#2568=ORIENTED_EDGE('',*,*,#1909,.F.);
#2569=ORIENTED_EDGE('',*,*,#1910,.F.);
#2570=ORIENTED_EDGE('',*,*,#1911,.T.);
#2571=ORIENTED_EDGE('',*,*,#1907,.T.);
#2572=ORIENTED_EDGE('',*,*,#1912,.F.);
#2573=ORIENTED_EDGE('',*,*,#1913,.F.);
#2574=ORIENTED_EDGE('',*,*,#1914,.T.);
#2575=ORIENTED_EDGE('',*,*,#1910,.T.);
#2576=ORIENTED_EDGE('',*,*,#1915,.F.);
#2577=ORIENTED_EDGE('',*,*,#1916,.F.);
#2578=ORIENTED_EDGE('',*,*,#1917,.T.);
#2579=ORIENTED_EDGE('',*,*,#1913,.T.);
#2580=ORIENTED_EDGE('',*,*,#1918,.F.);
#2581=ORIENTED_EDGE('',*,*,#1919,.F.);
#2582=ORIENTED_EDGE('',*,*,#1920,.T.);
#2583=ORIENTED_EDGE('',*,*,#1916,.T.);
#2584=ORIENTED_EDGE('',*,*,#1921,.F.);
#2585=ORIENTED_EDGE('',*,*,#1922,.F.);
#2586=ORIENTED_EDGE('',*,*,#1923,.T.);
#2587=ORIENTED_EDGE('',*,*,#1919,.T.);
#2588=ORIENTED_EDGE('',*,*,#1924,.F.);
#2589=ORIENTED_EDGE('',*,*,#1925,.F.);
#2590=ORIENTED_EDGE('',*,*,#1926,.T.);
#2591=ORIENTED_EDGE('',*,*,#1922,.T.);
#2592=ORIENTED_EDGE('',*,*,#1927,.F.);
#2593=ORIENTED_EDGE('',*,*,#1928,.F.);
#2594=ORIENTED_EDGE('',*,*,#1929,.F.);
#2595=ORIENTED_EDGE('',*,*,#1930,.F.);
#2596=ORIENTED_EDGE('',*,*,#1931,.F.);
#2597=ORIENTED_EDGE('',*,*,#1932,.F.);
#2598=ORIENTED_EDGE('',*,*,#1928,.T.);
#2599=ORIENTED_EDGE('',*,*,#1933,.F.);
#2600=ORIENTED_EDGE('',*,*,#1934,.T.);
#2601=ORIENTED_EDGE('',*,*,#1935,.T.);
#2602=ORIENTED_EDGE('',*,*,#1936,.F.);
#2603=ORIENTED_EDGE('',*,*,#1937,.F.);
#2604=ORIENTED_EDGE('',*,*,#1931,.T.);
#2605=ORIENTED_EDGE('',*,*,#1938,.T.);
#2606=ORIENTED_EDGE('',*,*,#1939,.F.);
#2607=ORIENTED_EDGE('',*,*,#1940,.F.);
#2608=ORIENTED_EDGE('',*,*,#1936,.T.);
#2609=ORIENTED_EDGE('',*,*,#1941,.T.);
#2610=ORIENTED_EDGE('',*,*,#1942,.F.);
#2611=ORIENTED_EDGE('',*,*,#1943,.F.);
#2612=ORIENTED_EDGE('',*,*,#1939,.T.);
#2613=ORIENTED_EDGE('',*,*,#1944,.T.);
#2614=ORIENTED_EDGE('',*,*,#1945,.F.);
#2615=ORIENTED_EDGE('',*,*,#1946,.F.);
#2616=ORIENTED_EDGE('',*,*,#1942,.T.);
#2617=ORIENTED_EDGE('',*,*,#1947,.T.);
#2618=ORIENTED_EDGE('',*,*,#1948,.F.);
#2619=ORIENTED_EDGE('',*,*,#1949,.F.);
#2620=ORIENTED_EDGE('',*,*,#1945,.T.);
#2621=ORIENTED_EDGE('',*,*,#1950,.T.);
#2622=ORIENTED_EDGE('',*,*,#1951,.F.);
#2623=ORIENTED_EDGE('',*,*,#1952,.F.);
#2624=ORIENTED_EDGE('',*,*,#1948,.T.);
#2625=ORIENTED_EDGE('',*,*,#1953,.T.);
#2626=ORIENTED_EDGE('',*,*,#1954,.F.);
#2627=ORIENTED_EDGE('',*,*,#1955,.F.);
#2628=ORIENTED_EDGE('',*,*,#1951,.T.);
#2629=ORIENTED_EDGE('',*,*,#1956,.T.);
#2630=ORIENTED_EDGE('',*,*,#1957,.F.);
#2631=ORIENTED_EDGE('',*,*,#1958,.F.);
#2632=ORIENTED_EDGE('',*,*,#1954,.T.);
#2633=ORIENTED_EDGE('',*,*,#1959,.T.);
#2634=ORIENTED_EDGE('',*,*,#1960,.F.);
#2635=ORIENTED_EDGE('',*,*,#1961,.F.);
#2636=ORIENTED_EDGE('',*,*,#1957,.T.);
#2637=ORIENTED_EDGE('',*,*,#1962,.T.);
#2638=ORIENTED_EDGE('',*,*,#1963,.F.);
#2639=ORIENTED_EDGE('',*,*,#1964,.F.);
#2640=ORIENTED_EDGE('',*,*,#1960,.T.);
#2641=ORIENTED_EDGE('',*,*,#1965,.T.);
#2642=ORIENTED_EDGE('',*,*,#1966,.F.);
#2643=ORIENTED_EDGE('',*,*,#1967,.F.);
#2644=ORIENTED_EDGE('',*,*,#1963,.T.);
#2645=ORIENTED_EDGE('',*,*,#1968,.T.);
#2646=ORIENTED_EDGE('',*,*,#1969,.F.);
#2647=ORIENTED_EDGE('',*,*,#1970,.F.);
#2648=ORIENTED_EDGE('',*,*,#1966,.T.);
#2649=ORIENTED_EDGE('',*,*,#1971,.T.);
#2650=ORIENTED_EDGE('',*,*,#1972,.F.);
#2651=ORIENTED_EDGE('',*,*,#1973,.F.);
#2652=ORIENTED_EDGE('',*,*,#1969,.T.);
#2653=ORIENTED_EDGE('',*,*,#1974,.T.);
#2654=ORIENTED_EDGE('',*,*,#1975,.F.);
#2655=ORIENTED_EDGE('',*,*,#1976,.F.);
#2656=ORIENTED_EDGE('',*,*,#1972,.T.);
#2657=ORIENTED_EDGE('',*,*,#1977,.T.);
#2658=ORIENTED_EDGE('',*,*,#1978,.F.);
#2659=ORIENTED_EDGE('',*,*,#1979,.F.);
#2660=ORIENTED_EDGE('',*,*,#1975,.T.);
#2661=ORIENTED_EDGE('',*,*,#1980,.T.);
#2662=ORIENTED_EDGE('',*,*,#1981,.F.);
#2663=ORIENTED_EDGE('',*,*,#1982,.F.);
#2664=ORIENTED_EDGE('',*,*,#1978,.T.);
#2665=ORIENTED_EDGE('',*,*,#1983,.T.);
#2666=ORIENTED_EDGE('',*,*,#1984,.F.);
#2667=ORIENTED_EDGE('',*,*,#1985,.F.);
#2668=ORIENTED_EDGE('',*,*,#1981,.T.);
#2669=ORIENTED_EDGE('',*,*,#1986,.T.);
#2670=ORIENTED_EDGE('',*,*,#1987,.F.);
#2671=ORIENTED_EDGE('',*,*,#1988,.F.);
#2672=ORIENTED_EDGE('',*,*,#1984,.T.);
#2673=ORIENTED_EDGE('',*,*,#1989,.T.);
#2674=ORIENTED_EDGE('',*,*,#1990,.F.);
#2675=ORIENTED_EDGE('',*,*,#1991,.F.);
#2676=ORIENTED_EDGE('',*,*,#1987,.T.);
#2677=ORIENTED_EDGE('',*,*,#1992,.T.);
#2678=ORIENTED_EDGE('',*,*,#1993,.F.);
#2679=ORIENTED_EDGE('',*,*,#1994,.F.);
#2680=ORIENTED_EDGE('',*,*,#1990,.T.);
#2681=ORIENTED_EDGE('',*,*,#1995,.T.);
#2682=ORIENTED_EDGE('',*,*,#1996,.F.);
#2683=ORIENTED_EDGE('',*,*,#1997,.F.);
#2684=ORIENTED_EDGE('',*,*,#1993,.T.);
#2685=ORIENTED_EDGE('',*,*,#1998,.T.);
#2686=ORIENTED_EDGE('',*,*,#1999,.F.);
#2687=ORIENTED_EDGE('',*,*,#2000,.F.);
#2688=ORIENTED_EDGE('',*,*,#1996,.T.);
#2689=ORIENTED_EDGE('',*,*,#2001,.T.);
#2690=ORIENTED_EDGE('',*,*,#2002,.F.);
#2691=ORIENTED_EDGE('',*,*,#2003,.F.);
#2692=ORIENTED_EDGE('',*,*,#1999,.T.);
#2693=ORIENTED_EDGE('',*,*,#2004,.T.);
#2694=ORIENTED_EDGE('',*,*,#2005,.F.);
#2695=ORIENTED_EDGE('',*,*,#2006,.F.);
#2696=ORIENTED_EDGE('',*,*,#2002,.T.);
#2697=ORIENTED_EDGE('',*,*,#2007,.T.);
#2698=ORIENTED_EDGE('',*,*,#2008,.T.);
#2699=ORIENTED_EDGE('',*,*,#2009,.T.);
#2700=ORIENTED_EDGE('',*,*,#2010,.T.);
#2701=ORIENTED_EDGE('',*,*,#2011,.T.);
#2702=ORIENTED_EDGE('',*,*,#2012,.F.);
#2703=ORIENTED_EDGE('',*,*,#2013,.T.);
#2704=ORIENTED_EDGE('',*,*,#2014,.T.);
#2705=ORIENTED_EDGE('',*,*,#2009,.F.);
#2706=ORIENTED_EDGE('',*,*,#2015,.T.);
#2707=ORIENTED_EDGE('',*,*,#2016,.T.);
#2708=ORIENTED_EDGE('',*,*,#2017,.F.);
#2709=ORIENTED_EDGE('',*,*,#2018,.F.);
#2710=ORIENTED_EDGE('',*,*,#2016,.F.);
#2711=ORIENTED_EDGE('',*,*,#2013,.F.);
#2712=ORIENTED_EDGE('',*,*,#2019,.F.);
#2713=ORIENTED_EDGE('',*,*,#2005,.T.);
#2714=ORIENTED_EDGE('',*,*,#2020,.T.);
#2715=ORIENTED_EDGE('',*,*,#2021,.T.);
#2716=ORIENTED_EDGE('',*,*,#2022,.T.);
#2717=ORIENTED_EDGE('',*,*,#2023,.F.);
#2718=ORIENTED_EDGE('',*,*,#2022,.F.);
#2719=ORIENTED_EDGE('',*,*,#2017,.T.);
#2720=ORIENTED_EDGE('',*,*,#2018,.T.);
#2721=ORIENTED_EDGE('',*,*,#2024,.T.);
#2722=ORIENTED_EDGE('',*,*,#2025,.F.);
#2723=ORIENTED_EDGE('',*,*,#2024,.F.);
#2724=ORIENTED_EDGE('',*,*,#2015,.F.);
#2725=ORIENTED_EDGE('',*,*,#2023,.T.);
#2726=ORIENTED_EDGE('',*,*,#2008,.F.);
#2727=ORIENTED_EDGE('',*,*,#2021,.F.);
#2728=ORIENTED_EDGE('',*,*,#2025,.T.);
#2729=ORIENTED_EDGE('',*,*,#1933,.T.);
#2730=ORIENTED_EDGE('',*,*,#1930,.T.);
#2731=ORIENTED_EDGE('',*,*,#2026,.F.);
#2732=ORIENTED_EDGE('',*,*,#2027,.F.);
#2733=ORIENTED_EDGE('',*,*,#2028,.F.);
#2734=ORIENTED_EDGE('',*,*,#1934,.F.);
#2735=ORIENTED_EDGE('',*,*,#2029,.F.);
#2736=ORIENTED_EDGE('',*,*,#2011,.F.);
#2737=ORIENTED_EDGE('',*,*,#2030,.F.);
#2738=ORIENTED_EDGE('',*,*,#1848,.F.);
#2739=ORIENTED_EDGE('',*,*,#2026,.T.);
#2740=ORIENTED_EDGE('',*,*,#1929,.T.);
#2741=ORIENTED_EDGE('',*,*,#1932,.T.);
#2742=ORIENTED_EDGE('',*,*,#1937,.T.);
#2743=ORIENTED_EDGE('',*,*,#1940,.T.);
#2744=ORIENTED_EDGE('',*,*,#1943,.T.);
#2745=ORIENTED_EDGE('',*,*,#1946,.T.);
#2746=ORIENTED_EDGE('',*,*,#1949,.T.);
#2747=ORIENTED_EDGE('',*,*,#1952,.T.);
#2748=ORIENTED_EDGE('',*,*,#1955,.T.);
#2749=ORIENTED_EDGE('',*,*,#1958,.T.);
#2750=ORIENTED_EDGE('',*,*,#1961,.T.);
#2751=ORIENTED_EDGE('',*,*,#1964,.T.);
#2752=ORIENTED_EDGE('',*,*,#1967,.T.);
#2753=ORIENTED_EDGE('',*,*,#1970,.T.);
#2754=ORIENTED_EDGE('',*,*,#1973,.T.);
#2755=ORIENTED_EDGE('',*,*,#1976,.T.);
#2756=ORIENTED_EDGE('',*,*,#1979,.T.);
#2757=ORIENTED_EDGE('',*,*,#1982,.T.);
#2758=ORIENTED_EDGE('',*,*,#1985,.T.);
#2759=ORIENTED_EDGE('',*,*,#1988,.T.);
#2760=ORIENTED_EDGE('',*,*,#1991,.T.);
#2761=ORIENTED_EDGE('',*,*,#1994,.T.);
#2762=ORIENTED_EDGE('',*,*,#1997,.T.);
#2763=ORIENTED_EDGE('',*,*,#2000,.T.);
#2764=ORIENTED_EDGE('',*,*,#2003,.T.);
#2765=ORIENTED_EDGE('',*,*,#2006,.T.);
#2766=ORIENTED_EDGE('',*,*,#2019,.T.);
#2767=ORIENTED_EDGE('',*,*,#2012,.T.);
#2768=ORIENTED_EDGE('',*,*,#2029,.T.);
#2769=ORIENTED_EDGE('',*,*,#1847,.F.);
#2770=ORIENTED_EDGE('',*,*,#1851,.F.);
#2771=ORIENTED_EDGE('',*,*,#1854,.F.);
#2772=ORIENTED_EDGE('',*,*,#1857,.F.);
#2773=ORIENTED_EDGE('',*,*,#1860,.F.);
#2774=ORIENTED_EDGE('',*,*,#1863,.F.);
#2775=ORIENTED_EDGE('',*,*,#1866,.F.);
#2776=ORIENTED_EDGE('',*,*,#1869,.F.);
#2777=ORIENTED_EDGE('',*,*,#1872,.F.);
#2778=ORIENTED_EDGE('',*,*,#1875,.F.);
#2779=ORIENTED_EDGE('',*,*,#1878,.F.);
#2780=ORIENTED_EDGE('',*,*,#1881,.F.);
#2781=ORIENTED_EDGE('',*,*,#1884,.F.);
#2782=ORIENTED_EDGE('',*,*,#1887,.F.);
#2783=ORIENTED_EDGE('',*,*,#1890,.F.);
#2784=ORIENTED_EDGE('',*,*,#1893,.F.);
#2785=ORIENTED_EDGE('',*,*,#1896,.F.);
#2786=ORIENTED_EDGE('',*,*,#1899,.F.);
#2787=ORIENTED_EDGE('',*,*,#1902,.F.);
#2788=ORIENTED_EDGE('',*,*,#1905,.F.);
#2789=ORIENTED_EDGE('',*,*,#1908,.F.);
#2790=ORIENTED_EDGE('',*,*,#1911,.F.);
#2791=ORIENTED_EDGE('',*,*,#1914,.F.);
#2792=ORIENTED_EDGE('',*,*,#1917,.F.);
#2793=ORIENTED_EDGE('',*,*,#1920,.F.);
#2794=ORIENTED_EDGE('',*,*,#1923,.F.);
#2795=ORIENTED_EDGE('',*,*,#1926,.F.);
#2796=ORIENTED_EDGE('',*,*,#2031,.F.);
#2797=ORIENTED_EDGE('',*,*,#1925,.T.);
#2798=ORIENTED_EDGE('',*,*,#2032,.F.);
#2799=ORIENTED_EDGE('',*,*,#2027,.T.);
#2800=ORIENTED_EDGE('',*,*,#2031,.T.);
#2801=ORIENTED_EDGE('',*,*,#2028,.T.);
#2802=ORIENTED_EDGE('',*,*,#2032,.T.);
#2803=ORIENTED_EDGE('',*,*,#1927,.T.);
#2804=ORIENTED_EDGE('',*,*,#1924,.T.);
#2805=ORIENTED_EDGE('',*,*,#1921,.T.);
#2806=ORIENTED_EDGE('',*,*,#1918,.T.);
#2807=ORIENTED_EDGE('',*,*,#1915,.T.);
#2808=ORIENTED_EDGE('',*,*,#1912,.T.);
#2809=ORIENTED_EDGE('',*,*,#1909,.T.);
#2810=ORIENTED_EDGE('',*,*,#1906,.T.);
#2811=ORIENTED_EDGE('',*,*,#1903,.T.);
#2812=ORIENTED_EDGE('',*,*,#1900,.T.);
#2813=ORIENTED_EDGE('',*,*,#1897,.T.);
#2814=ORIENTED_EDGE('',*,*,#1894,.T.);
#2815=ORIENTED_EDGE('',*,*,#1891,.T.);
#2816=ORIENTED_EDGE('',*,*,#1888,.T.);
#2817=ORIENTED_EDGE('',*,*,#1885,.T.);
#2818=ORIENTED_EDGE('',*,*,#1882,.T.);
#2819=ORIENTED_EDGE('',*,*,#1879,.T.);
#2820=ORIENTED_EDGE('',*,*,#1876,.T.);
#2821=ORIENTED_EDGE('',*,*,#1873,.T.);
#2822=ORIENTED_EDGE('',*,*,#1870,.T.);
#2823=ORIENTED_EDGE('',*,*,#1867,.T.);
#2824=ORIENTED_EDGE('',*,*,#1864,.T.);
#2825=ORIENTED_EDGE('',*,*,#1861,.T.);
#2826=ORIENTED_EDGE('',*,*,#1858,.T.);
#2827=ORIENTED_EDGE('',*,*,#1855,.T.);
#2828=ORIENTED_EDGE('',*,*,#1852,.T.);
#2829=ORIENTED_EDGE('',*,*,#1849,.T.);
#2830=ORIENTED_EDGE('',*,*,#2030,.T.);
#2831=ORIENTED_EDGE('',*,*,#2010,.F.);
#2832=ORIENTED_EDGE('',*,*,#2014,.F.);
#2833=ORIENTED_EDGE('',*,*,#2020,.F.);
#2834=ORIENTED_EDGE('',*,*,#2007,.F.);
#2835=ORIENTED_EDGE('',*,*,#2004,.F.);
#2836=ORIENTED_EDGE('',*,*,#2001,.F.);
#2837=ORIENTED_EDGE('',*,*,#1998,.F.);
#2838=ORIENTED_EDGE('',*,*,#1995,.F.);
#2839=ORIENTED_EDGE('',*,*,#1992,.F.);
#2840=ORIENTED_EDGE('',*,*,#1989,.F.);
#2841=ORIENTED_EDGE('',*,*,#1986,.F.);
#2842=ORIENTED_EDGE('',*,*,#1983,.F.);
#2843=ORIENTED_EDGE('',*,*,#1980,.F.);
#2844=ORIENTED_EDGE('',*,*,#1977,.F.);
#2845=ORIENTED_EDGE('',*,*,#1974,.F.);
#2846=ORIENTED_EDGE('',*,*,#1971,.F.);
#2847=ORIENTED_EDGE('',*,*,#1968,.F.);
#2848=ORIENTED_EDGE('',*,*,#1965,.F.);
#2849=ORIENTED_EDGE('',*,*,#1962,.F.);
#2850=ORIENTED_EDGE('',*,*,#1959,.F.);
#2851=ORIENTED_EDGE('',*,*,#1956,.F.);
#2852=ORIENTED_EDGE('',*,*,#1953,.F.);
#2853=ORIENTED_EDGE('',*,*,#1950,.F.);
#2854=ORIENTED_EDGE('',*,*,#1947,.F.);
#2855=ORIENTED_EDGE('',*,*,#1944,.F.);
#2856=ORIENTED_EDGE('',*,*,#1941,.F.);
#2857=ORIENTED_EDGE('',*,*,#1938,.F.);
#2858=ORIENTED_EDGE('',*,*,#1935,.F.);
#2859=ORIENTED_EDGE('',*,*,#2033,.F.);
#2860=ORIENTED_EDGE('',*,*,#2034,.T.);
#2861=ORIENTED_EDGE('',*,*,#2035,.T.);
#2862=ORIENTED_EDGE('',*,*,#2034,.F.);
#2863=ORIENTED_EDGE('',*,*,#2036,.F.);
#2864=ORIENTED_EDGE('',*,*,#2037,.F.);
#2865=ORIENTED_EDGE('',*,*,#2038,.T.);
#2866=ORIENTED_EDGE('',*,*,#2039,.F.);
#2867=ORIENTED_EDGE('',*,*,#2038,.F.);
#2868=ORIENTED_EDGE('',*,*,#2036,.T.);
#2869=ORIENTED_EDGE('',*,*,#2037,.T.);
#2870=ORIENTED_EDGE('',*,*,#2040,.T.);
#2871=ORIENTED_EDGE('',*,*,#2041,.F.);
#2872=ORIENTED_EDGE('',*,*,#2040,.F.);
#2873=ORIENTED_EDGE('',*,*,#2042,.T.);
#2874=ORIENTED_EDGE('',*,*,#2043,.T.);
#2875=ORIENTED_EDGE('',*,*,#2044,.F.);
#2876=ORIENTED_EDGE('',*,*,#2043,.F.);
#2877=ORIENTED_EDGE('',*,*,#2041,.T.);
#2878=ORIENTED_EDGE('',*,*,#2035,.F.);
#2879=ORIENTED_EDGE('',*,*,#2039,.T.);
#2880=ORIENTED_EDGE('',*,*,#2044,.T.);
#2881=ORIENTED_EDGE('',*,*,#2033,.T.);
#2882=ORIENTED_EDGE('',*,*,#2042,.F.);
#2883=ORIENTED_EDGE('',*,*,#2045,.T.);
#2884=ORIENTED_EDGE('',*,*,#2046,.T.);
#2885=ORIENTED_EDGE('',*,*,#2047,.F.);
#2886=ORIENTED_EDGE('',*,*,#2046,.F.);
#2887=ORIENTED_EDGE('',*,*,#2048,.T.);
#2888=ORIENTED_EDGE('',*,*,#2049,.T.);
#2889=ORIENTED_EDGE('',*,*,#2050,.F.);
#2890=ORIENTED_EDGE('',*,*,#2049,.F.);
#2891=ORIENTED_EDGE('',*,*,#2051,.T.);
#2892=ORIENTED_EDGE('',*,*,#2052,.F.);
#2893=ORIENTED_EDGE('',*,*,#2053,.T.);
#2894=ORIENTED_EDGE('',*,*,#2054,.T.);
#2895=ORIENTED_EDGE('',*,*,#2055,.F.);
#2896=ORIENTED_EDGE('',*,*,#2052,.T.);
#2897=ORIENTED_EDGE('',*,*,#2056,.T.);
#2898=ORIENTED_EDGE('',*,*,#2057,.F.);
#2899=ORIENTED_EDGE('',*,*,#2051,.F.);
#2900=ORIENTED_EDGE('',*,*,#2048,.F.);
#2901=ORIENTED_EDGE('',*,*,#2058,.F.);
#2902=ORIENTED_EDGE('',*,*,#2059,.F.);
#2903=ORIENTED_EDGE('',*,*,#2060,.T.);
#2904=ORIENTED_EDGE('',*,*,#2061,.T.);
#2905=ORIENTED_EDGE('',*,*,#2062,.F.);
#2906=ORIENTED_EDGE('',*,*,#2054,.F.);
#2907=ORIENTED_EDGE('',*,*,#2050,.T.);
#2908=ORIENTED_EDGE('',*,*,#2062,.T.);
#2909=ORIENTED_EDGE('',*,*,#2063,.T.);
#2910=ORIENTED_EDGE('',*,*,#2064,.F.);
#2911=ORIENTED_EDGE('',*,*,#2065,.T.);
#2912=ORIENTED_EDGE('',*,*,#2056,.F.);
#2913=ORIENTED_EDGE('',*,*,#2055,.T.);
#2914=ORIENTED_EDGE('',*,*,#2047,.T.);
#2915=ORIENTED_EDGE('',*,*,#2066,.T.);
#2916=ORIENTED_EDGE('',*,*,#2060,.F.);
#2917=ORIENTED_EDGE('',*,*,#2053,.F.);
#2918=ORIENTED_EDGE('',*,*,#2059,.T.);
#2919=ORIENTED_EDGE('',*,*,#2067,.T.);
#2920=ORIENTED_EDGE('',*,*,#2068,.T.);
#2921=ORIENTED_EDGE('',*,*,#2045,.F.);
#2922=ORIENTED_EDGE('',*,*,#2064,.T.);
#2923=ORIENTED_EDGE('',*,*,#2069,.T.);
#2924=ORIENTED_EDGE('',*,*,#2068,.F.);
#2925=ORIENTED_EDGE('',*,*,#2070,.T.);
#2926=ORIENTED_EDGE('',*,*,#2065,.F.);
#2927=ORIENTED_EDGE('',*,*,#2070,.F.);
#2928=ORIENTED_EDGE('',*,*,#2067,.F.);
#2929=ORIENTED_EDGE('',*,*,#2058,.T.);
#2930=ORIENTED_EDGE('',*,*,#2057,.T.);
#2931=ORIENTED_EDGE('',*,*,#2066,.F.);
#2932=ORIENTED_EDGE('',*,*,#2069,.F.);
#2933=ORIENTED_EDGE('',*,*,#2063,.F.);
#2934=ORIENTED_EDGE('',*,*,#2061,.F.);
#2935=ORIENTED_EDGE('',*,*,#2071,.T.);
#2936=ORIENTED_EDGE('',*,*,#2072,.T.);
#2937=ORIENTED_EDGE('',*,*,#2073,.T.);
#2938=ORIENTED_EDGE('',*,*,#2072,.F.);
#2939=ORIENTED_EDGE('',*,*,#2074,.F.);
#2940=ORIENTED_EDGE('',*,*,#2075,.T.);
#2941=ORIENTED_EDGE('',*,*,#2076,.T.);
#2942=ORIENTED_EDGE('',*,*,#2075,.F.);
#2943=ORIENTED_EDGE('',*,*,#2077,.T.);
#2944=ORIENTED_EDGE('',*,*,#2078,.T.);
#2945=ORIENTED_EDGE('',*,*,#2079,.T.);
#2946=ORIENTED_EDGE('',*,*,#2078,.F.);
#2947=ORIENTED_EDGE('',*,*,#2080,.F.);
#2948=ORIENTED_EDGE('',*,*,#2081,.T.);
#2949=ORIENTED_EDGE('',*,*,#2082,.T.);
#2950=ORIENTED_EDGE('',*,*,#2081,.F.);
#2951=ORIENTED_EDGE('',*,*,#2083,.F.);
#2952=ORIENTED_EDGE('',*,*,#2084,.F.);
#2953=ORIENTED_EDGE('',*,*,#2085,.F.);
#2954=ORIENTED_EDGE('',*,*,#2086,.F.);
#2955=ORIENTED_EDGE('',*,*,#2087,.T.);
#2956=ORIENTED_EDGE('',*,*,#2088,.F.);
#2957=ORIENTED_EDGE('',*,*,#2089,.F.);
#2958=ORIENTED_EDGE('',*,*,#2090,.F.);
#2959=ORIENTED_EDGE('',*,*,#2091,.T.);
#2960=ORIENTED_EDGE('',*,*,#2092,.F.);
#2961=ORIENTED_EDGE('',*,*,#2093,.F.);
#2962=ORIENTED_EDGE('',*,*,#2094,.T.);
#2963=ORIENTED_EDGE('',*,*,#2092,.T.);
#2964=ORIENTED_EDGE('',*,*,#2095,.F.);
#2965=ORIENTED_EDGE('',*,*,#2096,.F.);
#2966=ORIENTED_EDGE('',*,*,#2097,.T.);
#2967=ORIENTED_EDGE('',*,*,#2098,.T.);
#2968=ORIENTED_EDGE('',*,*,#2096,.T.);
#2969=ORIENTED_EDGE('',*,*,#2099,.F.);
#2970=ORIENTED_EDGE('',*,*,#2100,.T.);
#2971=ORIENTED_EDGE('',*,*,#2101,.T.);
#2972=ORIENTED_EDGE('',*,*,#2102,.T.);
#2973=ORIENTED_EDGE('',*,*,#2103,.F.);
#2974=ORIENTED_EDGE('',*,*,#2104,.F.);
#2975=ORIENTED_EDGE('',*,*,#2105,.F.);
#2976=ORIENTED_EDGE('',*,*,#2084,.T.);
#2977=ORIENTED_EDGE('',*,*,#2106,.T.);
#2978=ORIENTED_EDGE('',*,*,#2104,.T.);
#2979=ORIENTED_EDGE('',*,*,#2107,.F.);
#2980=ORIENTED_EDGE('',*,*,#2086,.T.);
#2981=ORIENTED_EDGE('',*,*,#2108,.T.);
#2982=ORIENTED_EDGE('',*,*,#2094,.F.);
#2983=ORIENTED_EDGE('',*,*,#2097,.F.);
#2984=ORIENTED_EDGE('',*,*,#2098,.F.);
#2985=ORIENTED_EDGE('',*,*,#2106,.F.);
#2986=ORIENTED_EDGE('',*,*,#2083,.T.);
#2987=ORIENTED_EDGE('',*,*,#2107,.T.);
#2988=ORIENTED_EDGE('',*,*,#2093,.T.);
#2989=ORIENTED_EDGE('',*,*,#2073,.F.);
#2990=ORIENTED_EDGE('',*,*,#2079,.F.);
#2991=ORIENTED_EDGE('',*,*,#2109,.F.);
#2992=ORIENTED_EDGE('',*,*,#2087,.F.);
#2993=ORIENTED_EDGE('',*,*,#2108,.F.);
#2994=ORIENTED_EDGE('',*,*,#2085,.T.);
#2995=ORIENTED_EDGE('',*,*,#2105,.T.);
#2996=ORIENTED_EDGE('',*,*,#2103,.T.);
#2997=ORIENTED_EDGE('',*,*,#2071,.F.);
#2998=ORIENTED_EDGE('',*,*,#2077,.F.);
#2999=ORIENTED_EDGE('',*,*,#2088,.T.);
#3000=ORIENTED_EDGE('',*,*,#2109,.T.);
#3001=ORIENTED_EDGE('',*,*,#2102,.F.);
#3002=ORIENTED_EDGE('',*,*,#2110,.F.);
#3003=ORIENTED_EDGE('',*,*,#2111,.T.);
#3004=ORIENTED_EDGE('',*,*,#2100,.F.);
#3005=ORIENTED_EDGE('',*,*,#2112,.F.);
#3006=ORIENTED_EDGE('',*,*,#2113,.F.);
#3007=ORIENTED_EDGE('',*,*,#2114,.T.);
#3008=ORIENTED_EDGE('',*,*,#2090,.T.);
#3009=ORIENTED_EDGE('',*,*,#2115,.F.);
#3010=ORIENTED_EDGE('',*,*,#2116,.F.);
#3011=ORIENTED_EDGE('',*,*,#2112,.T.);
#3012=ORIENTED_EDGE('',*,*,#2099,.T.);
#3013=ORIENTED_EDGE('',*,*,#2095,.T.);
#3014=ORIENTED_EDGE('',*,*,#2091,.F.);
#3015=ORIENTED_EDGE('',*,*,#2114,.F.);
#3016=ORIENTED_EDGE('',*,*,#2117,.F.);
#3017=ORIENTED_EDGE('',*,*,#2074,.T.);
#3018=ORIENTED_EDGE('',*,*,#2080,.T.);
#3019=ORIENTED_EDGE('',*,*,#2089,.T.);
#3020=ORIENTED_EDGE('',*,*,#2110,.T.);
#3021=ORIENTED_EDGE('',*,*,#2101,.F.);
#3022=ORIENTED_EDGE('',*,*,#2111,.F.);
#3023=ORIENTED_EDGE('',*,*,#2118,.F.);
#3024=ORIENTED_EDGE('',*,*,#2115,.T.);
#3025=ORIENTED_EDGE('',*,*,#2076,.F.);
#3026=ORIENTED_EDGE('',*,*,#2082,.F.);
#3027=ORIENTED_EDGE('',*,*,#2116,.T.);
#3028=ORIENTED_EDGE('',*,*,#2118,.T.);
#3029=ORIENTED_EDGE('',*,*,#2113,.T.);
#3030=ORIENTED_EDGE('',*,*,#2117,.T.);
#3031=ORIENTED_EDGE('',*,*,#2119,.T.);
#3032=ORIENTED_EDGE('',*,*,#2120,.T.);
#3033=ORIENTED_EDGE('',*,*,#2121,.T.);
#3034=ORIENTED_EDGE('',*,*,#2122,.F.);
#3035=ORIENTED_EDGE('',*,*,#2123,.T.);
#3036=ORIENTED_EDGE('',*,*,#2124,.F.);
#3037=ORIENTED_EDGE('',*,*,#2125,.T.);
#3038=ORIENTED_EDGE('',*,*,#2123,.F.);
#3039=ORIENTED_EDGE('',*,*,#2120,.F.);
#3040=ORIENTED_EDGE('',*,*,#2126,.T.);
#3041=ORIENTED_EDGE('',*,*,#2124,.T.);
#3042=ORIENTED_EDGE('',*,*,#2122,.T.);
#3043=ORIENTED_EDGE('',*,*,#2127,.T.);
#3044=ORIENTED_EDGE('',*,*,#2127,.F.);
#3045=ORIENTED_EDGE('',*,*,#2121,.F.);
#3046=ORIENTED_EDGE('',*,*,#2119,.F.);
#3047=ORIENTED_EDGE('',*,*,#2125,.F.);
#3048=ORIENTED_EDGE('',*,*,#2126,.F.);
#3049=ORIENTED_EDGE('',*,*,#2128,.T.);
#3050=ORIENTED_EDGE('',*,*,#2129,.T.);
#3051=ORIENTED_EDGE('',*,*,#2130,.T.);
#3052=ORIENTED_EDGE('',*,*,#2131,.T.);
#3053=ORIENTED_EDGE('',*,*,#2129,.F.);
#3054=ORIENTED_EDGE('',*,*,#2132,.T.);
#3055=ORIENTED_EDGE('',*,*,#2133,.T.);
#3056=ORIENTED_EDGE('',*,*,#2130,.F.);
#3057=ORIENTED_EDGE('',*,*,#2131,.F.);
#3058=ORIENTED_EDGE('',*,*,#2133,.F.);
#3059=ORIENTED_EDGE('',*,*,#2134,.T.);
#3060=ORIENTED_EDGE('',*,*,#2135,.T.);
#3061=ORIENTED_EDGE('',*,*,#2136,.T.);
#3062=ORIENTED_EDGE('',*,*,#2137,.T.);
#3063=ORIENTED_EDGE('',*,*,#2136,.F.);
#3064=ORIENTED_EDGE('',*,*,#2138,.T.);
#3065=ORIENTED_EDGE('',*,*,#2139,.T.);
#3066=ORIENTED_EDGE('',*,*,#2140,.T.);
#3067=ORIENTED_EDGE('',*,*,#2141,.T.);
#3068=ORIENTED_EDGE('',*,*,#2142,.T.);
#3069=ORIENTED_EDGE('',*,*,#2143,.T.);
#3070=ORIENTED_EDGE('',*,*,#2144,.T.);
#3071=ORIENTED_EDGE('',*,*,#2145,.T.);
#3072=ORIENTED_EDGE('',*,*,#2146,.T.);
#3073=ORIENTED_EDGE('',*,*,#2147,.T.);
#3074=ORIENTED_EDGE('',*,*,#2139,.F.);
#3075=ORIENTED_EDGE('',*,*,#2148,.T.);
#3076=ORIENTED_EDGE('',*,*,#2138,.F.);
#3077=ORIENTED_EDGE('',*,*,#2149,.T.);
#3078=ORIENTED_EDGE('',*,*,#2150,.T.);
#3079=ORIENTED_EDGE('',*,*,#2149,.F.);
#3080=ORIENTED_EDGE('',*,*,#2148,.F.);
#3081=ORIENTED_EDGE('',*,*,#2132,.F.);
#3082=ORIENTED_EDGE('',*,*,#2151,.T.);
#3083=ORIENTED_EDGE('',*,*,#2135,.F.);
#3084=ORIENTED_EDGE('',*,*,#2151,.F.);
#3085=ORIENTED_EDGE('',*,*,#2134,.F.);
#3086=ORIENTED_EDGE('',*,*,#2152,.F.);
#3087=ORIENTED_EDGE('',*,*,#2153,.T.);
#3088=ORIENTED_EDGE('',*,*,#2154,.T.);
#3089=ORIENTED_EDGE('',*,*,#2155,.T.);
#3090=ORIENTED_EDGE('',*,*,#2156,.T.);
#3091=ORIENTED_EDGE('',*,*,#2157,.F.);
#3092=ORIENTED_EDGE('',*,*,#2158,.T.);
#3093=ORIENTED_EDGE('',*,*,#2152,.T.);
#3094=ORIENTED_EDGE('',*,*,#2159,.T.);
#3095=ORIENTED_EDGE('',*,*,#2160,.T.);
#3096=ORIENTED_EDGE('',*,*,#2161,.F.);
#3097=ORIENTED_EDGE('',*,*,#2162,.T.);
#3098=ORIENTED_EDGE('',*,*,#2157,.T.);
#3099=ORIENTED_EDGE('',*,*,#2163,.F.);
#3100=ORIENTED_EDGE('',*,*,#2164,.F.);
#3101=ORIENTED_EDGE('',*,*,#2165,.F.);
#3102=ORIENTED_EDGE('',*,*,#2166,.T.);
#3103=ORIENTED_EDGE('',*,*,#2161,.T.);
#3104=ORIENTED_EDGE('',*,*,#2167,.T.);
#3105=ORIENTED_EDGE('',*,*,#2168,.T.);
#3106=ORIENTED_EDGE('',*,*,#2169,.F.);
#3107=ORIENTED_EDGE('',*,*,#2170,.T.);
#3108=ORIENTED_EDGE('',*,*,#2165,.T.);
#3109=ORIENTED_EDGE('',*,*,#2171,.T.);
#3110=ORIENTED_EDGE('',*,*,#2172,.T.);
#3111=ORIENTED_EDGE('',*,*,#2154,.F.);
#3112=ORIENTED_EDGE('',*,*,#2173,.T.);
#3113=ORIENTED_EDGE('',*,*,#2169,.T.);
#3114=ORIENTED_EDGE('',*,*,#2174,.T.);
#3115=ORIENTED_EDGE('',*,*,#2175,.T.);
#3116=ORIENTED_EDGE('',*,*,#2176,.T.);
#3117=ORIENTED_EDGE('',*,*,#2177,.T.);
#3118=ORIENTED_EDGE('',*,*,#2178,.T.);
#3119=ORIENTED_EDGE('',*,*,#2179,.T.);
#3120=ORIENTED_EDGE('',*,*,#2180,.T.);
#3121=ORIENTED_EDGE('',*,*,#2181,.T.);
#3122=ORIENTED_EDGE('',*,*,#2137,.F.);
#3123=ORIENTED_EDGE('',*,*,#2150,.F.);
#3124=ORIENTED_EDGE('',*,*,#2128,.F.);
#3125=ORIENTED_EDGE('',*,*,#2164,.T.);
#3126=ORIENTED_EDGE('',*,*,#2176,.F.);
#3127=ORIENTED_EDGE('',*,*,#2167,.F.);
#3128=ORIENTED_EDGE('',*,*,#2181,.F.);
#3129=ORIENTED_EDGE('',*,*,#2171,.F.);
#3130=ORIENTED_EDGE('',*,*,#2168,.F.);
#3131=ORIENTED_EDGE('',*,*,#2180,.F.);
#3132=ORIENTED_EDGE('',*,*,#2174,.F.);
#3133=ORIENTED_EDGE('',*,*,#2172,.F.);
#3134=ORIENTED_EDGE('',*,*,#2175,.F.);
#3135=ORIENTED_EDGE('',*,*,#2179,.F.);
#3136=ORIENTED_EDGE('',*,*,#2155,.F.);
#3137=ORIENTED_EDGE('',*,*,#2178,.F.);
#3138=ORIENTED_EDGE('',*,*,#2159,.F.);
#3139=ORIENTED_EDGE('',*,*,#2156,.F.);
#3140=ORIENTED_EDGE('',*,*,#2177,.F.);
#3141=ORIENTED_EDGE('',*,*,#2163,.T.);
#3142=ORIENTED_EDGE('',*,*,#2160,.F.);
#3143=ORIENTED_EDGE('',*,*,#2182,.F.);
#3144=ORIENTED_EDGE('',*,*,#2142,.F.);
#3145=ORIENTED_EDGE('',*,*,#2183,.F.);
#3146=ORIENTED_EDGE('',*,*,#2170,.F.);
#3147=ORIENTED_EDGE('',*,*,#2183,.T.);
#3148=ORIENTED_EDGE('',*,*,#2141,.F.);
#3149=ORIENTED_EDGE('',*,*,#2184,.F.);
#3150=ORIENTED_EDGE('',*,*,#2166,.F.);
#3151=ORIENTED_EDGE('',*,*,#2182,.T.);
#3152=ORIENTED_EDGE('',*,*,#2173,.F.);
#3153=ORIENTED_EDGE('',*,*,#2185,.F.);
#3154=ORIENTED_EDGE('',*,*,#2144,.F.);
#3155=ORIENTED_EDGE('',*,*,#2143,.F.);
#3156=ORIENTED_EDGE('',*,*,#2184,.T.);
#3157=ORIENTED_EDGE('',*,*,#2140,.F.);
#3158=ORIENTED_EDGE('',*,*,#2147,.F.);
#3159=ORIENTED_EDGE('',*,*,#2186,.F.);
#3160=ORIENTED_EDGE('',*,*,#2162,.F.);
#3161=ORIENTED_EDGE('',*,*,#2185,.T.);
#3162=ORIENTED_EDGE('',*,*,#2153,.F.);
#3163=ORIENTED_EDGE('',*,*,#2187,.F.);
#3164=ORIENTED_EDGE('',*,*,#2145,.F.);
#3165=ORIENTED_EDGE('',*,*,#2186,.T.);
#3166=ORIENTED_EDGE('',*,*,#2146,.F.);
#3167=ORIENTED_EDGE('',*,*,#2187,.T.);
#3168=ORIENTED_EDGE('',*,*,#2158,.F.);
#3169=ORIENTED_EDGE('',*,*,#2188,.T.);
#3170=ORIENTED_EDGE('',*,*,#2189,.T.);
#3171=ORIENTED_EDGE('',*,*,#2190,.F.);
#3172=ORIENTED_EDGE('',*,*,#2189,.F.);
#3173=ORIENTED_EDGE('',*,*,#2191,.T.);
#3174=ORIENTED_EDGE('',*,*,#2192,.T.);
#3175=ORIENTED_EDGE('',*,*,#2193,.F.);
#3176=ORIENTED_EDGE('',*,*,#2192,.F.);
#3177=ORIENTED_EDGE('',*,*,#2194,.F.);
#3178=ORIENTED_EDGE('',*,*,#2195,.T.);
#3179=ORIENTED_EDGE('',*,*,#2196,.F.);
#3180=ORIENTED_EDGE('',*,*,#2195,.F.);
#3181=ORIENTED_EDGE('',*,*,#2193,.T.);
#3182=ORIENTED_EDGE('',*,*,#2191,.F.);
#3183=ORIENTED_EDGE('',*,*,#2194,.T.);
#3184=ORIENTED_EDGE('',*,*,#2190,.T.);
#3185=ORIENTED_EDGE('',*,*,#2188,.F.);
#3186=ORIENTED_EDGE('',*,*,#2196,.T.);
#3187=CYLINDRICAL_SURFACE('',#3576,30.);
#3188=CYLINDRICAL_SURFACE('',#3579,40.);
#3189=CYLINDRICAL_SURFACE('',#3584,40.);
#3190=CYLINDRICAL_SURFACE('',#3598,2.);
#3191=CYLINDRICAL_SURFACE('',#3601,6.);
#3192=CYLINDRICAL_SURFACE('',#3604,6.);
#3193=CYLINDRICAL_SURFACE('',#3607,12.5);
#3194=CYLINDRICAL_SURFACE('',#3610,12.5);
#3195=CYLINDRICAL_SURFACE('',#3630,12.5);
#3196=CYLINDRICAL_SURFACE('',#3644,12.5);
#3197=CYLINDRICAL_SURFACE('',#3648,10.);
#3198=CYLINDRICAL_SURFACE('',#3650,5.75643035625);
#3199=CYLINDRICAL_SURFACE('',#3651,5.75643035625);
#3200=CYLINDRICAL_SURFACE('',#3652,5.75643035625);
#3201=CYLINDRICAL_SURFACE('',#3653,5.75643035625);
#3202=CYLINDRICAL_SURFACE('',#3654,5.75643035625);
#3203=CYLINDRICAL_SURFACE('',#3655,5.75643035625);
#3204=CYLINDRICAL_SURFACE('',#3656,5.75643035625);
#3205=CYLINDRICAL_SURFACE('',#3657,5.75643035625);
#3206=CYLINDRICAL_SURFACE('',#3658,5.75643035625);
#3207=CYLINDRICAL_SURFACE('',#3659,5.75643035625);
#3208=CYLINDRICAL_SURFACE('',#3660,5.75643035625);
#3209=CYLINDRICAL_SURFACE('',#3661,5.75643035625);
#3210=CYLINDRICAL_SURFACE('',#3662,5.75643035625);
#3211=CYLINDRICAL_SURFACE('',#3663,5.75643035625);
#3212=CYLINDRICAL_SURFACE('',#3664,5.75643035625);
#3213=CYLINDRICAL_SURFACE('',#3665,5.75643035625);
#3214=CYLINDRICAL_SURFACE('',#3666,5.75643035625);
#3215=CYLINDRICAL_SURFACE('',#3667,5.75643035625);
#3216=CYLINDRICAL_SURFACE('',#3668,5.75643035625);
#3217=CYLINDRICAL_SURFACE('',#3669,5.75643035625);
#3218=CYLINDRICAL_SURFACE('',#3670,5.75643035625);
#3219=CYLINDRICAL_SURFACE('',#3671,5.75643035625);
#3220=CYLINDRICAL_SURFACE('',#3672,5.75643035625);
#3221=CYLINDRICAL_SURFACE('',#3673,5.75643035625);
#3222=CYLINDRICAL_SURFACE('',#3674,5.75643035625);
#3223=CYLINDRICAL_SURFACE('',#3675,5.75643035625);
#3224=CYLINDRICAL_SURFACE('',#3676,5.75643035625);
#3225=CYLINDRICAL_SURFACE('',#3677,6.);
#3226=CYLINDRICAL_SURFACE('',#3679,6.);
#3227=CYLINDRICAL_SURFACE('',#3681,6.);
#3228=CYLINDRICAL_SURFACE('',#3682,6.);
#3229=CYLINDRICAL_SURFACE('',#3683,6.);
#3230=CYLINDRICAL_SURFACE('',#3684,6.);
#3231=CYLINDRICAL_SURFACE('',#3685,6.);
#3232=CYLINDRICAL_SURFACE('',#3686,6.);
#3233=CYLINDRICAL_SURFACE('',#3687,6.);
#3234=CYLINDRICAL_SURFACE('',#3688,6.);
#3235=CYLINDRICAL_SURFACE('',#3689,6.);
#3236=CYLINDRICAL_SURFACE('',#3690,6.);
#3237=CYLINDRICAL_SURFACE('',#3691,6.);
#3238=CYLINDRICAL_SURFACE('',#3692,6.);
#3239=CYLINDRICAL_SURFACE('',#3693,6.);
#3240=CYLINDRICAL_SURFACE('',#3694,6.);
#3241=CYLINDRICAL_SURFACE('',#3695,6.);
#3242=CYLINDRICAL_SURFACE('',#3696,6.);
#3243=CYLINDRICAL_SURFACE('',#3697,6.);
#3244=CYLINDRICAL_SURFACE('',#3698,6.);
#3245=CYLINDRICAL_SURFACE('',#3699,6.);
#3246=CYLINDRICAL_SURFACE('',#3700,6.);
#3247=CYLINDRICAL_SURFACE('',#3701,6.);
#3248=CYLINDRICAL_SURFACE('',#3702,6.);
#3249=CYLINDRICAL_SURFACE('',#3703,6.);
#3250=CYLINDRICAL_SURFACE('',#3704,6.);
#3251=CYLINDRICAL_SURFACE('',#3705,6.);
#3252=CYLINDRICAL_SURFACE('',#3712,6.);
#3253=CYLINDRICAL_SURFACE('',#3713,9.);
#3254=CYLINDRICAL_SURFACE('',#3716,6.);
#3255=CYLINDRICAL_SURFACE('',#3724,5.75643035625);
#3256=CYLINDRICAL_SURFACE('',#3726,15.);
#3257=CYLINDRICAL_SURFACE('',#3733,30.);
#3258=CYLINDRICAL_SURFACE('',#3735,6.);
#3259=CYLINDRICAL_SURFACE('',#3742,2.);
#3260=CYLINDRICAL_SURFACE('',#3745,6.25);
#3261=CYLINDRICAL_SURFACE('',#3749,11.25);
#3262=CYLINDRICAL_SURFACE('',#3761,5.);
#3263=CYLINDRICAL_SURFACE('',#3762,3.);
#3264=CYLINDRICAL_SURFACE('',#3764,2.);
#3265=CYLINDRICAL_SURFACE('',#3767,2.);
#3266=CYLINDRICAL_SURFACE('',#3770,2.);
#3267=CYLINDRICAL_SURFACE('',#3773,2.);
#3268=CYLINDRICAL_SURFACE('',#3776,4.);
#3269=CYLINDRICAL_SURFACE('',#3793,4.);
#3270=CYLINDRICAL_SURFACE('',#3803,6.);
#3271=CYLINDRICAL_SURFACE('',#3819,5.1);
#3272=CYLINDRICAL_SURFACE('',#3841,3.);
#3273=CYLINDRICAL_SURFACE('',#3844,3.);
#3274=CYLINDRICAL_SURFACE('',#3847,1.9);
#3275=ADVANCED_FACE('',(#365),#3187,.F.);
#3276=ADVANCED_FACE('',(#366),#3188,.T.);
#3277=ADVANCED_FACE('',(#367,#257),#285,.T.);
#3278=ADVANCED_FACE('',(#368),#3189,.T.);
#3279=ADVANCED_FACE('',(#369,#258),#286,.F.);
#3280=ADVANCED_FACE('',(#370),#287,.F.);
#3281=ADVANCED_FACE('',(#371),#288,.F.);
#3282=ADVANCED_FACE('',(#372),#289,.F.);
#3283=ADVANCED_FACE('',(#373),#290,.F.);
#3284=ADVANCED_FACE('',(#374),#291,.T.);
#3285=ADVANCED_FACE('',(#375),#292,.F.);
#3286=ADVANCED_FACE('',(#376),#293,.F.);
#3287=ADVANCED_FACE('',(#377),#294,.F.);
#3288=ADVANCED_FACE('',(#378),#295,.F.);
#3289=ADVANCED_FACE('',(#379),#296,.F.);
#3290=ADVANCED_FACE('',(#380),#3190,.F.);
#3291=ADVANCED_FACE('',(#381),#3191,.F.);
#3292=ADVANCED_FACE('',(#382),#3192,.F.);
#3293=ADVANCED_FACE('',(#383),#3193,.T.);
#3294=ADVANCED_FACE('',(#384),#3194,.T.);
#3295=ADVANCED_FACE('',(#385),#297,.F.);
#3296=ADVANCED_FACE('',(#386),#298,.F.);
#3297=ADVANCED_FACE('',(#387,#259),#299,.T.);
#3298=ADVANCED_FACE('',(#388),#300,.F.);
#3299=ADVANCED_FACE('',(#389),#301,.T.);
#3300=ADVANCED_FACE('',(#390),#302,.T.);
#3301=ADVANCED_FACE('',(#391),#303,.F.);
#3302=ADVANCED_FACE('',(#392),#304,.F.);
#3303=ADVANCED_FACE('',(#393),#305,.T.);
#3304=ADVANCED_FACE('',(#394),#306,.F.);
#3305=ADVANCED_FACE('',(#395),#307,.T.);
#3306=ADVANCED_FACE('',(#396,#260),#308,.F.);
#3307=ADVANCED_FACE('',(#397),#309,.T.);
#3308=ADVANCED_FACE('',(#398,#261),#310,.T.);
#3309=ADVANCED_FACE('',(#399),#3195,.T.);
#3310=ADVANCED_FACE('',(#400),#311,.F.);
#3311=ADVANCED_FACE('',(#401),#312,.F.);
#3312=ADVANCED_FACE('',(#402),#313,.F.);
#3313=ADVANCED_FACE('',(#403,#262),#314,.F.);
#3314=ADVANCED_FACE('',(#404,#263),#315,.T.);
#3315=ADVANCED_FACE('',(#405,#264),#316,.F.);
#3316=ADVANCED_FACE('',(#406),#317,.F.);
#3317=ADVANCED_FACE('',(#407),#318,.F.);
#3318=ADVANCED_FACE('',(#408),#319,.T.);
#3319=ADVANCED_FACE('',(#409),#320,.T.);
#3320=ADVANCED_FACE('',(#410),#3196,.T.);
#3321=ADVANCED_FACE('',(#411),#321,.F.);
#3322=ADVANCED_FACE('',(#412),#322,.F.);
#3323=ADVANCED_FACE('',(#413),#323,.T.);
#3324=ADVANCED_FACE('',(#414),#3197,.T.);
#3325=ADVANCED_FACE('',(#415),#3198,.T.);
#3326=ADVANCED_FACE('',(#416),#3199,.T.);
#3327=ADVANCED_FACE('',(#417),#3200,.T.);
#3328=ADVANCED_FACE('',(#418),#3201,.T.);
#3329=ADVANCED_FACE('',(#419),#3202,.T.);
#3330=ADVANCED_FACE('',(#420),#3203,.T.);
#3331=ADVANCED_FACE('',(#421),#3204,.T.);
#3332=ADVANCED_FACE('',(#422),#3205,.T.);
#3333=ADVANCED_FACE('',(#423),#3206,.T.);
#3334=ADVANCED_FACE('',(#424),#3207,.T.);
#3335=ADVANCED_FACE('',(#425),#3208,.T.);
#3336=ADVANCED_FACE('',(#426),#3209,.T.);
#3337=ADVANCED_FACE('',(#427),#3210,.T.);
#3338=ADVANCED_FACE('',(#428),#3211,.T.);
#3339=ADVANCED_FACE('',(#429),#3212,.T.);
#3340=ADVANCED_FACE('',(#430),#3213,.T.);
#3341=ADVANCED_FACE('',(#431),#3214,.T.);
#3342=ADVANCED_FACE('',(#432),#3215,.T.);
#3343=ADVANCED_FACE('',(#433),#3216,.T.);
#3344=ADVANCED_FACE('',(#434),#3217,.T.);
#3345=ADVANCED_FACE('',(#435),#3218,.T.);
#3346=ADVANCED_FACE('',(#436),#3219,.T.);
#3347=ADVANCED_FACE('',(#437),#3220,.T.);
#3348=ADVANCED_FACE('',(#438),#3221,.T.);
#3349=ADVANCED_FACE('',(#439),#3222,.T.);
#3350=ADVANCED_FACE('',(#440),#3223,.T.);
#3351=ADVANCED_FACE('',(#441),#3224,.T.);
#3352=ADVANCED_FACE('',(#442),#3225,.T.);
#3353=ADVANCED_FACE('',(#443),#3226,.T.);
#3354=ADVANCED_FACE('',(#444),#3227,.T.);
#3355=ADVANCED_FACE('',(#445),#3228,.T.);
#3356=ADVANCED_FACE('',(#446),#3229,.T.);
#3357=ADVANCED_FACE('',(#447),#3230,.T.);
#3358=ADVANCED_FACE('',(#448),#3231,.T.);
#3359=ADVANCED_FACE('',(#449),#3232,.T.);
#3360=ADVANCED_FACE('',(#450),#3233,.T.);
#3361=ADVANCED_FACE('',(#451),#3234,.T.);
#3362=ADVANCED_FACE('',(#452),#3235,.T.);
#3363=ADVANCED_FACE('',(#453),#3236,.T.);
#3364=ADVANCED_FACE('',(#454),#3237,.T.);
#3365=ADVANCED_FACE('',(#455),#3238,.T.);
#3366=ADVANCED_FACE('',(#456),#3239,.T.);
#3367=ADVANCED_FACE('',(#457),#3240,.T.);
#3368=ADVANCED_FACE('',(#458),#3241,.T.);
#3369=ADVANCED_FACE('',(#459),#3242,.T.);
#3370=ADVANCED_FACE('',(#460),#3243,.T.);
#3371=ADVANCED_FACE('',(#461),#3244,.T.);
#3372=ADVANCED_FACE('',(#462),#3245,.T.);
#3373=ADVANCED_FACE('',(#463),#3246,.T.);
#3374=ADVANCED_FACE('',(#464),#3247,.T.);
#3375=ADVANCED_FACE('',(#465),#3248,.T.);
#3376=ADVANCED_FACE('',(#466),#3249,.T.);
#3377=ADVANCED_FACE('',(#467),#3250,.T.);
#3378=ADVANCED_FACE('',(#468),#3251,.T.);
#3379=ADVANCED_FACE('',(#469),#71,.T.);
#3380=ADVANCED_FACE('',(#470),#3252,.T.);
#3381=ADVANCED_FACE('',(#471),#3253,.T.);
#3382=ADVANCED_FACE('',(#472),#3254,.T.);
#3383=ADVANCED_FACE('',(#473),#324,.F.);
#3384=ADVANCED_FACE('',(#474,#265),#325,.T.);
#3385=ADVANCED_FACE('',(#475,#266),#326,.F.);
#3386=ADVANCED_FACE('',(#476),#327,.T.);
#3387=ADVANCED_FACE('',(#477),#328,.F.);
#3388=ADVANCED_FACE('',(#478),#329,.T.);
#3389=ADVANCED_FACE('',(#479),#61,.T.);
#3390=ADVANCED_FACE('',(#480),#3255,.T.);
#3391=ADVANCED_FACE('',(#481),#62,.T.);
#3392=ADVANCED_FACE('',(#482),#3256,.F.);
#3393=ADVANCED_FACE('',(#483),#51,.T.);
#3394=ADVANCED_FACE('',(#484),#3257,.T.);
#3395=ADVANCED_FACE('',(#485),#3258,.F.);
#3396=ADVANCED_FACE('',(#486,#267),#330,.T.);
#3397=ADVANCED_FACE('',(#487,#268),#331,.F.);
#3398=ADVANCED_FACE('',(#488,#269),#332,.T.);
#3399=ADVANCED_FACE('',(#489),#3259,.F.);
#3400=ADVANCED_FACE('',(#490),#3260,.F.);
#3401=ADVANCED_FACE('',(#491),#3261,.T.);
#3402=ADVANCED_FACE('',(#492),#333,.T.);
#3403=ADVANCED_FACE('',(#493,#270),#334,.F.);
#3404=ADVANCED_FACE('',(#494,#271),#335,.F.);
#3405=ADVANCED_FACE('',(#495,#272),#336,.T.);
#3406=ADVANCED_FACE('',(#496),#337,.F.);
#3407=ADVANCED_FACE('',(#497),#3262,.T.);
#3408=ADVANCED_FACE('',(#498),#3263,.T.);
#3409=ADVANCED_FACE('',(#499),#3264,.F.);
#3410=ADVANCED_FACE('',(#500),#3265,.F.);
#3411=ADVANCED_FACE('',(#501),#3266,.F.);
#3412=ADVANCED_FACE('',(#502),#3267,.F.);
#3413=ADVANCED_FACE('',(#503),#3268,.T.);
#3414=ADVANCED_FACE('',(#504),#338,.F.);
#3415=ADVANCED_FACE('',(#505),#339,.T.);
#3416=ADVANCED_FACE('',(#506),#340,.T.);
#3417=ADVANCED_FACE('',(#507),#341,.T.);
#3418=ADVANCED_FACE('',(#508),#342,.F.);
#3419=ADVANCED_FACE('',(#509,#273,#274),#343,.F.);
#3420=ADVANCED_FACE('',(#510,#275,#276),#344,.T.);
#3421=ADVANCED_FACE('',(#511),#345,.T.);
#3422=ADVANCED_FACE('',(#512),#346,.T.);
#3423=ADVANCED_FACE('',(#513),#347,.F.);
#3424=ADVANCED_FACE('',(#514,#277,#278),#348,.F.);
#3425=ADVANCED_FACE('',(#515,#279,#280),#349,.T.);
#3426=ADVANCED_FACE('',(#516),#3269,.T.);
#3427=ADVANCED_FACE('',(#517),#63,.T.);
#3428=ADVANCED_FACE('',(#518),#350,.T.);
#3429=ADVANCED_FACE('',(#519),#64,.T.);
#3430=ADVANCED_FACE('',(#520),#351,.F.);
#3431=ADVANCED_FACE('',(#521),#352,.T.);
#3432=ADVANCED_FACE('',(#522),#3270,.F.);
#3433=ADVANCED_FACE('',(#523),#52,.F.);
#3434=ADVANCED_FACE('',(#524),#53,.F.);
#3435=ADVANCED_FACE('',(#525),#54,.T.);
#3436=ADVANCED_FACE('',(#526),#72,.T.);
#3437=ADVANCED_FACE('',(#527),#3271,.F.);
#3438=ADVANCED_FACE('',(#528),#353,.T.);
#3439=ADVANCED_FACE('',(#529),#354,.T.);
#3440=ADVANCED_FACE('',(#530),#355,.F.);
#3441=ADVANCED_FACE('',(#531),#356,.T.);
#3442=ADVANCED_FACE('',(#532),#357,.T.);
#3443=ADVANCED_FACE('',(#533),#358,.T.);
#3444=ADVANCED_FACE('',(#534,#281),#359,.T.);
#3445=ADVANCED_FACE('',(#535,#282),#360,.F.);
#3446=ADVANCED_FACE('',(#536),#55,.T.);
#3447=ADVANCED_FACE('',(#537),#56,.T.);
#3448=ADVANCED_FACE('',(#538),#57,.T.);
#3449=ADVANCED_FACE('',(#539),#58,.T.);
#3450=ADVANCED_FACE('',(#540),#59,.T.);
#3451=ADVANCED_FACE('',(#541),#60,.T.);
#3452=ADVANCED_FACE('',(#542),#65,.F.);
#3453=ADVANCED_FACE('',(#543),#66,.F.);
#3454=ADVANCED_FACE('',(#544),#67,.F.);
#3455=ADVANCED_FACE('',(#545),#68,.F.);
#3456=ADVANCED_FACE('',(#546),#69,.F.);
#3457=ADVANCED_FACE('',(#547),#70,.F.);
#3458=ADVANCED_FACE('',(#548),#3272,.T.);
#3459=ADVANCED_FACE('',(#549),#3273,.T.);
#3460=ADVANCED_FACE('',(#550),#3274,.T.);
#3461=ADVANCED_FACE('',(#551),#361,.T.);
#3462=ADVANCED_FACE('',(#552,#283),#362,.F.);
#3463=ADVANCED_FACE('',(#553),#363,.T.);
#3464=ADVANCED_FACE('',(#554,#284),#364,.F.);
#3465=CLOSED_SHELL('',(#3275,#3276,#3277,#3278,#3279,#3280,#3281,#3282,
#3283,#3284,#3285,#3286,#3287,#3288,#3289));
#3466=CLOSED_SHELL('',(#3290,#3291,#3292,#3293,#3294,#3295,#3296,#3297,
#3298,#3299,#3300,#3301,#3302,#3303,#3304,#3305,#3306,#3307,#3308,#3309,
#3310,#3311,#3312,#3313,#3314,#3315,#3316,#3317,#3318,#3319,#3320,#3321,
#3322,#3323,#3324));
#3467=CLOSED_SHELL('',(#3325,#3326,#3327,#3328,#3329,#3330,#3331,#3332,
#3333,#3334,#3335,#3336,#3337,#3338,#3339,#3340,#3341,#3342,#3343,#3344,
#3345,#3346,#3347,#3348,#3349,#3350,#3351,#3352,#3353,#3354,#3355,#3356,
#3357,#3358,#3359,#3360,#3361,#3362,#3363,#3364,#3365,#3366,#3367,#3368,
#3369,#3370,#3371,#3372,#3373,#3374,#3375,#3376,#3377,#3378,#3379,#3380,
#3381,#3382,#3383,#3384,#3385,#3386,#3387,#3388,#3389,#3390,#3391));
#3468=CLOSED_SHELL('',(#3392,#3393,#3394,#3395,#3396,#3397,#3398));
#3469=CLOSED_SHELL('',(#3399,#3400,#3401,#3402,#3403,#3404,#3405,#3406,
#3407,#3408));
#3470=CLOSED_SHELL('',(#3409,#3410,#3411,#3412,#3413,#3414,#3415,#3416,
#3417,#3418,#3419,#3420,#3421,#3422,#3423,#3424,#3425,#3426));
#3471=CLOSED_SHELL('',(#3427,#3428,#3429,#3430,#3431));
#3472=CLOSED_SHELL('',(#3432,#3433,#3434,#3435,#3436,#3437,#3438,#3439,
#3440,#3441,#3442,#3443,#3444,#3445,#3446,#3447,#3448,#3449,#3450,#3451,
#3452,#3453,#3454,#3455,#3456,#3457));
#3473=CLOSED_SHELL('',(#3458,#3459,#3460,#3461,#3462,#3463,#3464));
#3474=DERIVED_UNIT_ELEMENT(#3492,1.);
#3475=DERIVED_UNIT_ELEMENT(#14086,-3.);
#3476=DERIVED_UNIT_ELEMENT(#3492,1.);
#3477=DERIVED_UNIT_ELEMENT(#14086,-3.);
#3478=DERIVED_UNIT_ELEMENT(#3492,1.);
#3479=DERIVED_UNIT_ELEMENT(#14086,-3.);
#3480=DERIVED_UNIT_ELEMENT(#3492,1.);
#3481=DERIVED_UNIT_ELEMENT(#14086,-3.);
#3482=DERIVED_UNIT_ELEMENT(#3492,1.);
#3483=DERIVED_UNIT_ELEMENT(#14086,-3.);
#3484=DERIVED_UNIT_ELEMENT(#3492,1.);
#3485=DERIVED_UNIT_ELEMENT(#14086,-3.);
#3486=DERIVED_UNIT_ELEMENT(#3492,1.);
#3487=DERIVED_UNIT_ELEMENT(#14086,-3.);
#3488=DERIVED_UNIT_ELEMENT(#3492,1.);
#3489=DERIVED_UNIT_ELEMENT(#14086,-3.);
#3490=DERIVED_UNIT_ELEMENT(#3492,1.);
#3491=DERIVED_UNIT_ELEMENT(#14086,-3.);
#3492=(
MASS_UNIT()
NAMED_UNIT(*)
SI_UNIT(.KILO.,.GRAM.)
);
#3493=DERIVED_UNIT((#3474,#3475));
#3494=DERIVED_UNIT((#3476,#3477));
#3495=DERIVED_UNIT((#3478,#3479));
#3496=DERIVED_UNIT((#3480,#3481));
#3497=DERIVED_UNIT((#3482,#3483));
#3498=DERIVED_UNIT((#3484,#3485));
#3499=DERIVED_UNIT((#3486,#3487));
#3500=DERIVED_UNIT((#3488,#3489));
#3501=DERIVED_UNIT((#3490,#3491));
#3502=MEASURE_REPRESENTATION_ITEM('density measure',
POSITIVE_RATIO_MEASURE(7850.),#3493);
#3503=MEASURE_REPRESENTATION_ITEM('density measure',
POSITIVE_RATIO_MEASURE(7850.),#3494);
#3504=MEASURE_REPRESENTATION_ITEM('density measure',
POSITIVE_RATIO_MEASURE(7850.),#3495);
#3505=MEASURE_REPRESENTATION_ITEM('density measure',
POSITIVE_RATIO_MEASURE(7850.),#3496);
#3506=MEASURE_REPRESENTATION_ITEM('density measure',
POSITIVE_RATIO_MEASURE(7850.),#3497);
#3507=MEASURE_REPRESENTATION_ITEM('density measure',
POSITIVE_RATIO_MEASURE(7850.),#3498);
#3508=MEASURE_REPRESENTATION_ITEM('density measure',
POSITIVE_RATIO_MEASURE(7850.),#3499);
#3509=MEASURE_REPRESENTATION_ITEM('density measure',
POSITIVE_RATIO_MEASURE(7850.),#3500);
#3510=MEASURE_REPRESENTATION_ITEM('density measure',
POSITIVE_RATIO_MEASURE(7850.),#3501);
#3511=PROPERTY_DEFINITION_REPRESENTATION(#3556,#3529);
#3512=PROPERTY_DEFINITION_REPRESENTATION(#3557,#3530);
#3513=PROPERTY_DEFINITION_REPRESENTATION(#3558,#3531);
#3514=PROPERTY_DEFINITION_REPRESENTATION(#3559,#3532);
#3515=PROPERTY_DEFINITION_REPRESENTATION(#3560,#3533);
#3516=PROPERTY_DEFINITION_REPRESENTATION(#3561,#3534);
#3517=PROPERTY_DEFINITION_REPRESENTATION(#3562,#3535);
#3518=PROPERTY_DEFINITION_REPRESENTATION(#3563,#3536);
#3519=PROPERTY_DEFINITION_REPRESENTATION(#3564,#3537);
#3520=PROPERTY_DEFINITION_REPRESENTATION(#3565,#3538);
#3521=PROPERTY_DEFINITION_REPRESENTATION(#3566,#3539);
#3522=PROPERTY_DEFINITION_REPRESENTATION(#3567,#3540);
#3523=PROPERTY_DEFINITION_REPRESENTATION(#3568,#3541);
#3524=PROPERTY_DEFINITION_REPRESENTATION(#3569,#3542);
#3525=PROPERTY_DEFINITION_REPRESENTATION(#3570,#3543);
#3526=PROPERTY_DEFINITION_REPRESENTATION(#3571,#3544);
#3527=PROPERTY_DEFINITION_REPRESENTATION(#3572,#3545);
#3528=PROPERTY_DEFINITION_REPRESENTATION(#3573,#3546);
#3529=REPRESENTATION('material name',(#3547),#14075);
#3530=REPRESENTATION('density',(#3502),#14075);
#3531=REPRESENTATION('material name',(#3548),#14076);
#3532=REPRESENTATION('density',(#3503),#14076);
#3533=REPRESENTATION('material name',(#3549),#14077);
#3534=REPRESENTATION('density',(#3504),#14077);
#3535=REPRESENTATION('material name',(#3550),#14078);
#3536=REPRESENTATION('density',(#3505),#14078);
#3537=REPRESENTATION('material name',(#3551),#14079);
#3538=REPRESENTATION('density',(#3506),#14079);
#3539=REPRESENTATION('material name',(#3552),#14080);
#3540=REPRESENTATION('density',(#3507),#14080);
#3541=REPRESENTATION('material name',(#3553),#14081);
#3542=REPRESENTATION('density',(#3508),#14081);
#3543=REPRESENTATION('material name',(#3554),#14082);
#3544=REPRESENTATION('density',(#3509),#14082);
#3545=REPRESENTATION('material name',(#3555),#14083);
#3546=REPRESENTATION('density',(#3510),#14083);
#3547=DESCRIPTIVE_REPRESENTATION_ITEM('Steel','Steel');
#3548=DESCRIPTIVE_REPRESENTATION_ITEM('Steel','Steel');
#3549=DESCRIPTIVE_REPRESENTATION_ITEM('Steel','Steel');
#3550=DESCRIPTIVE_REPRESENTATION_ITEM('Steel','Steel');
#3551=DESCRIPTIVE_REPRESENTATION_ITEM('Steel','Steel');
#3552=DESCRIPTIVE_REPRESENTATION_ITEM('Steel','Steel');
#3553=DESCRIPTIVE_REPRESENTATION_ITEM('Steel','Steel');
#3554=DESCRIPTIVE_REPRESENTATION_ITEM('Steel','Steel');
#3555=DESCRIPTIVE_REPRESENTATION_ITEM('Steel','Steel');
#3556=PROPERTY_DEFINITION('material property','material name',#14131);
#3557=PROPERTY_DEFINITION('material property','density of part',#14131);
#3558=PROPERTY_DEFINITION('material property','material name',#14132);
#3559=PROPERTY_DEFINITION('material property','density of part',#14132);
#3560=PROPERTY_DEFINITION('material property','material name',#14133);
#3561=PROPERTY_DEFINITION('material property','density of part',#14133);
#3562=PROPERTY_DEFINITION('material property','material name',#14134);
#3563=PROPERTY_DEFINITION('material property','density of part',#14134);
#3564=PROPERTY_DEFINITION('material property','material name',#14135);
#3565=PROPERTY_DEFINITION('material property','density of part',#14135);
#3566=PROPERTY_DEFINITION('material property','material name',#14136);
#3567=PROPERTY_DEFINITION('material property','density of part',#14136);
#3568=PROPERTY_DEFINITION('material property','material name',#14137);
#3569=PROPERTY_DEFINITION('material property','density of part',#14137);
#3570=PROPERTY_DEFINITION('material property','material name',#14138);
#3571=PROPERTY_DEFINITION('material property','density of part',#14138);
#3572=PROPERTY_DEFINITION('material property','material name',#14139);
#3573=PROPERTY_DEFINITION('material property','density of part',#14139);
#3574=AXIS2_PLACEMENT_3D('',#4701,#3864,#3865);
#3575=AXIS2_PLACEMENT_3D('',#4702,#3866,#3867);
#3576=AXIS2_PLACEMENT_3D('',#4703,#3868,#3869);
#3577=AXIS2_PLACEMENT_3D('',#4705,#3870,#3871);
#3578=AXIS2_PLACEMENT_3D('',#4708,#3873,#3874);
#3579=AXIS2_PLACEMENT_3D('',#4709,#3875,#3876);
#3580=AXIS2_PLACEMENT_3D('',#4712,#3877,#3878);
#3581=AXIS2_PLACEMENT_3D('',#4716,#3880,#3881);
#3582=AXIS2_PLACEMENT_3D('',#4718,#3883,#3884);
#3583=AXIS2_PLACEMENT_3D('',#4726,#3888,#3889);
#3584=AXIS2_PLACEMENT_3D('',#4732,#3893,#3894);
#3585=AXIS2_PLACEMENT_3D('',#4736,#3896,#3897);
#3586=AXIS2_PLACEMENT_3D('',#4738,#3899,#3900);
#3587=AXIS2_PLACEMENT_3D('',#4749,#3907,#3908);
#3588=AXIS2_PLACEMENT_3D('',#4755,#3912,#3913);
#3589=AXIS2_PLACEMENT_3D('',#4759,#3916,#3917);
#3590=AXIS2_PLACEMENT_3D('',#4763,#3920,#3921);
#3591=AXIS2_PLACEMENT_3D('',#4765,#3923,#3924);
#3592=AXIS2_PLACEMENT_3D('',#4766,#3925,#3926);
#3593=AXIS2_PLACEMENT_3D('',#4772,#3930,#3931);
#3594=AXIS2_PLACEMENT_3D('',#4776,#3934,#3935);
#3595=AXIS2_PLACEMENT_3D('',#4780,#3938,#3939);
#3596=AXIS2_PLACEMENT_3D('',#4782,#3941,#3942);
#3597=AXIS2_PLACEMENT_3D('',#4783,#3943,#3944);
#3598=AXIS2_PLACEMENT_3D('',#4784,#3945,#3946);
#3599=AXIS2_PLACEMENT_3D('',#4786,#3947,#3948);
#3600=AXIS2_PLACEMENT_3D('',#4789,#3950,#3951);
#3601=AXIS2_PLACEMENT_3D('',#4790,#3952,#3953);
#3602=AXIS2_PLACEMENT_3D('',#4792,#3954,#3955);
#3603=AXIS2_PLACEMENT_3D('',#4795,#3957,#3958);
#3604=AXIS2_PLACEMENT_3D('',#4796,#3959,#3960);
#3605=AXIS2_PLACEMENT_3D('',#4798,#3961,#3962);
#3606=AXIS2_PLACEMENT_3D('',#4801,#3964,#3965);
#3607=AXIS2_PLACEMENT_3D('',#4802,#3966,#3967);
#3608=AXIS2_PLACEMENT_3D('',#4805,#3968,#3969);
#3609=AXIS2_PLACEMENT_3D('',#4809,#3971,#3972);
#3610=AXIS2_PLACEMENT_3D('',#4811,#3974,#3975);
#3611=AXIS2_PLACEMENT_3D('',#4814,#3976,#3977);
#3612=AXIS2_PLACEMENT_3D('',#4818,#3979,#3980);
#3613=AXIS2_PLACEMENT_3D('',#4820,#3982,#3983);
#3614=AXIS2_PLACEMENT_3D('',#4845,#3996,#3997);
#3615=AXIS2_PLACEMENT_3D('',#4851,#4001,#4002);
#3616=AXIS2_PLACEMENT_3D('',#4859,#4006,#4007);
#3617=AXIS2_PLACEMENT_3D('',#4873,#4015,#4016);
#3618=AXIS2_PLACEMENT_3D('',#4877,#4019,#4020);
#3619=AXIS2_PLACEMENT_3D('',#4883,#4024,#4025);
#3620=AXIS2_PLACEMENT_3D('',#4897,#4033,#4034);
#3621=AXIS2_PLACEMENT_3D('',#4912,#4043,#4044);
#3622=AXIS2_PLACEMENT_3D('',#4915,#4047,#4048);
#3623=AXIS2_PLACEMENT_3D('',#4921,#4052,#4053);
#3624=AXIS2_PLACEMENT_3D('',#4924,#4056,#4057);
#3625=AXIS2_PLACEMENT_3D('',#4930,#4061,#4062);
#3626=AXIS2_PLACEMENT_3D('',#4931,#4063,#4064);
#3627=AXIS2_PLACEMENT_3D('',#4932,#4065,#4066);
#3628=AXIS2_PLACEMENT_3D('',#4938,#4070,#4071);
#3629=AXIS2_PLACEMENT_3D('',#4941,#4074,#4075);
#3630=AXIS2_PLACEMENT_3D('',#4943,#4077,#4078);
#3631=AXIS2_PLACEMENT_3D('',#4944,#4079,#4080);
#3632=AXIS2_PLACEMENT_3D('',#4946,#4082,#4083);
#3633=AXIS2_PLACEMENT_3D('',#4947,#4084,#4085);
#3634=AXIS2_PLACEMENT_3D('',#4948,#4086,#4087);
#3635=AXIS2_PLACEMENT_3D('',#4952,#4089,#4090);
#3636=AXIS2_PLACEMENT_3D('',#4962,#4097,#4098);
#3637=AXIS2_PLACEMENT_3D('',#4964,#4099,#4100);
#3638=AXIS2_PLACEMENT_3D('',#4978,#4109,#4110);
#3639=AXIS2_PLACEMENT_3D('',#4980,#4112,#4113);
#3640=AXIS2_PLACEMENT_3D('',#4981,#4114,#4115);
#3641=AXIS2_PLACEMENT_3D('',#4983,#4117,#4118);
#3642=AXIS2_PLACEMENT_3D('',#4985,#4120,#4121);
#3643=AXIS2_PLACEMENT_3D('',#4987,#4123,#4124);
#3644=AXIS2_PLACEMENT_3D('',#4988,#4125,#4126);
#3645=AXIS2_PLACEMENT_3D('',#4989,#4127,#4128);
#3646=AXIS2_PLACEMENT_3D('',#4990,#4129,#4130);
#3647=AXIS2_PLACEMENT_3D('',#4991,#4131,#4132);
#3648=AXIS2_PLACEMENT_3D('',#4993,#4134,#4135);
#3649=AXIS2_PLACEMENT_3D('',#4994,#4136,#4137);
#3650=AXIS2_PLACEMENT_3D('',#4995,#4138,#4139);
#3651=AXIS2_PLACEMENT_3D('',#5008,#4142,#4143);
#3652=AXIS2_PLACEMENT_3D('',#5038,#4145,#4146);
#3653=AXIS2_PLACEMENT_3D('',#5068,#4148,#4149);
#3654=AXIS2_PLACEMENT_3D('',#5098,#4151,#4152);
#3655=AXIS2_PLACEMENT_3D('',#5128,#4154,#4155);
#3656=AXIS2_PLACEMENT_3D('',#5158,#4157,#4158);
#3657=AXIS2_PLACEMENT_3D('',#5188,#4160,#4161);
#3658=AXIS2_PLACEMENT_3D('',#5218,#4163,#4164);
#3659=AXIS2_PLACEMENT_3D('',#5248,#4166,#4167);
#3660=AXIS2_PLACEMENT_3D('',#5278,#4169,#4170);
#3661=AXIS2_PLACEMENT_3D('',#5308,#4172,#4173);
#3662=AXIS2_PLACEMENT_3D('',#5338,#4175,#4176);
#3663=AXIS2_PLACEMENT_3D('',#5368,#4178,#4179);
#3664=AXIS2_PLACEMENT_3D('',#5398,#4181,#4182);
#3665=AXIS2_PLACEMENT_3D('',#5428,#4184,#4185);
#3666=AXIS2_PLACEMENT_3D('',#5458,#4187,#4188);
#3667=AXIS2_PLACEMENT_3D('',#5488,#4190,#4191);
#3668=AXIS2_PLACEMENT_3D('',#5518,#4193,#4194);
#3669=AXIS2_PLACEMENT_3D('',#5548,#4196,#4197);
#3670=AXIS2_PLACEMENT_3D('',#5578,#4199,#4200);
#3671=AXIS2_PLACEMENT_3D('',#5608,#4202,#4203);
#3672=AXIS2_PLACEMENT_3D('',#5638,#4205,#4206);
#3673=AXIS2_PLACEMENT_3D('',#5668,#4208,#4209);
#3674=AXIS2_PLACEMENT_3D('',#5698,#4211,#4212);
#3675=AXIS2_PLACEMENT_3D('',#5728,#4214,#4215);
#3676=AXIS2_PLACEMENT_3D('',#5758,#4217,#4218);
#3677=AXIS2_PLACEMENT_3D('',#5788,#4220,#4221);
#3678=AXIS2_PLACEMENT_3D('',#5805,#4223,#4224);
#3679=AXIS2_PLACEMENT_3D('',#5806,#4225,#4226);
#3680=AXIS2_PLACEMENT_3D('',#5846,#4228,#4229);
#3681=AXIS2_PLACEMENT_3D('',#5861,#4231,#4232);
#3682=AXIS2_PLACEMENT_3D('',#5937,#4234,#4235);
#3683=AXIS2_PLACEMENT_3D('',#6015,#4237,#4238);
#3684=AXIS2_PLACEMENT_3D('',#6093,#4240,#4241);
#3685=AXIS2_PLACEMENT_3D('',#6169,#4243,#4244);
#3686=AXIS2_PLACEMENT_3D('',#6245,#4246,#4247);
#3687=AXIS2_PLACEMENT_3D('',#6321,#4249,#4250);
#3688=AXIS2_PLACEMENT_3D('',#6399,#4252,#4253);
#3689=AXIS2_PLACEMENT_3D('',#6475,#4255,#4256);
#3690=AXIS2_PLACEMENT_3D('',#6553,#4258,#4259);
#3691=AXIS2_PLACEMENT_3D('',#6629,#4261,#4262);
#3692=AXIS2_PLACEMENT_3D('',#6705,#4264,#4265);
#3693=AXIS2_PLACEMENT_3D('',#6781,#4267,#4268);
#3694=AXIS2_PLACEMENT_3D('',#6857,#4270,#4271);
#3695=AXIS2_PLACEMENT_3D('',#6935,#4273,#4274);
#3696=AXIS2_PLACEMENT_3D('',#7013,#4276,#4277);
#3697=AXIS2_PLACEMENT_3D('',#7089,#4279,#4280);
#3698=AXIS2_PLACEMENT_3D('',#7165,#4282,#4283);
#3699=AXIS2_PLACEMENT_3D('',#7241,#4285,#4286);
#3700=AXIS2_PLACEMENT_3D('',#7319,#4288,#4289);
#3701=AXIS2_PLACEMENT_3D('',#7397,#4291,#4292);
#3702=AXIS2_PLACEMENT_3D('',#7473,#4294,#4295);
#3703=AXIS2_PLACEMENT_3D('',#7549,#4297,#4298);
#3704=AXIS2_PLACEMENT_3D('',#7625,#4300,#4301);
#3705=AXIS2_PLACEMENT_3D('',#7701,#4303,#4304);
#3706=AXIS2_PLACEMENT_3D('',#7703,#4305,#4306);
#3707=AXIS2_PLACEMENT_3D('',#7782,#4310,#4311);
#3708=AXIS2_PLACEMENT_3D('',#7784,#4312,#4313);
#3709=AXIS2_PLACEMENT_3D('',#7786,#4314,#4315);
#3710=AXIS2_PLACEMENT_3D('',#7788,#4316,#4317);
#3711=AXIS2_PLACEMENT_3D('',#7789,#4318,#4319);
#3712=AXIS2_PLACEMENT_3D('',#7790,#4320,#4321);
#3713=AXIS2_PLACEMENT_3D('',#7865,#4322,#4323);
#3714=AXIS2_PLACEMENT_3D('',#7867,#4324,#4325);
#3715=AXIS2_PLACEMENT_3D('',#7870,#4327,#4328);
#3716=AXIS2_PLACEMENT_3D('',#7871,#4329,#4330);
#3717=AXIS2_PLACEMENT_3D('',#7874,#4332,#4333);
#3718=AXIS2_PLACEMENT_3D('',#7875,#4334,#4335);
#3719=AXIS2_PLACEMENT_3D('',#7876,#4336,#4337);
#3720=AXIS2_PLACEMENT_3D('',#7877,#4338,#4339);
#3721=AXIS2_PLACEMENT_3D('',#7878,#4340,#4341);
#3722=AXIS2_PLACEMENT_3D('',#7879,#4342,#4343);
#3723=AXIS2_PLACEMENT_3D('',#7885,#4347,#4348);
#3724=AXIS2_PLACEMENT_3D('',#8537,#4351,#4352);
#3725=AXIS2_PLACEMENT_3D('',#9187,#4353,#4354);
#3726=AXIS2_PLACEMENT_3D('',#9188,#4355,#4356);
#3727=AXIS2_PLACEMENT_3D('',#9190,#4357,#4358);
#3728=AXIS2_PLACEMENT_3D('',#9193,#4360,#4361);
#3729=AXIS2_PLACEMENT_3D('',#9194,#4362,#4363);
#3730=AXIS2_PLACEMENT_3D('',#9197,#4364,#4365);
#3731=AXIS2_PLACEMENT_3D('',#9198,#4366,#4367);
#3732=AXIS2_PLACEMENT_3D('',#9201,#4369,#4370);
#3733=AXIS2_PLACEMENT_3D('',#9202,#4371,#4372);
#3734=AXIS2_PLACEMENT_3D('',#9205,#4374,#4375);
#3735=AXIS2_PLACEMENT_3D('',#9206,#4376,#4377);
#3736=AXIS2_PLACEMENT_3D('',#9208,#4378,#4379);
#3737=AXIS2_PLACEMENT_3D('',#9211,#4381,#4382);
#3738=AXIS2_PLACEMENT_3D('',#9212,#4383,#4384);
#3739=AXIS2_PLACEMENT_3D('',#9213,#4385,#4386);
#3740=AXIS2_PLACEMENT_3D('',#9214,#4387,#4388);
#3741=AXIS2_PLACEMENT_3D('',#9215,#4389,#4390);
#3742=AXIS2_PLACEMENT_3D('',#9216,#4391,#4392);
#3743=AXIS2_PLACEMENT_3D('',#9218,#4393,#4394);
#3744=AXIS2_PLACEMENT_3D('',#9221,#4396,#4397);
#3745=AXIS2_PLACEMENT_3D('',#9222,#4398,#4399);
#3746=AXIS2_PLACEMENT_3D('',#9225,#4400,#4401);
#3747=AXIS2_PLACEMENT_3D('',#9228,#4403,#4404);
#3748=AXIS2_PLACEMENT_3D('',#9229,#4405,#4406);
#3749=AXIS2_PLACEMENT_3D('',#9230,#4407,#4408);
#3750=AXIS2_PLACEMENT_3D('',#9233,#4409,#4410);
#3751=AXIS2_PLACEMENT_3D('',#9237,#4412,#4413);
#3752=AXIS2_PLACEMENT_3D('',#9239,#4415,#4416);
#3753=AXIS2_PLACEMENT_3D('',#9246,#4421,#4422);
#3754=AXIS2_PLACEMENT_3D('',#9252,#4426,#4427);
#3755=AXIS2_PLACEMENT_3D('',#9254,#4428,#4429);
#3756=AXIS2_PLACEMENT_3D('',#9257,#4431,#4432);
#3757=AXIS2_PLACEMENT_3D('',#9258,#4433,#4434);
#3758=AXIS2_PLACEMENT_3D('',#9260,#4435,#4436);
#3759=AXIS2_PLACEMENT_3D('',#9262,#4437,#4438);
#3760=AXIS2_PLACEMENT_3D('',#9264,#4440,#4441);
#3761=AXIS2_PLACEMENT_3D('',#9267,#4444,#4445);
#3762=AXIS2_PLACEMENT_3D('',#9268,#4446,#4447);
#3763=AXIS2_PLACEMENT_3D('',#9269,#4448,#4449);
#3764=AXIS2_PLACEMENT_3D('',#9270,#4450,#4451);
#3765=AXIS2_PLACEMENT_3D('',#9272,#4452,#4453);
#3766=AXIS2_PLACEMENT_3D('',#9275,#4455,#4456);
#3767=AXIS2_PLACEMENT_3D('',#9276,#4457,#4458);
#3768=AXIS2_PLACEMENT_3D('',#9278,#4459,#4460);
#3769=AXIS2_PLACEMENT_3D('',#9281,#4462,#4463);
#3770=AXIS2_PLACEMENT_3D('',#9282,#4464,#4465);
#3771=AXIS2_PLACEMENT_3D('',#9284,#4466,#4467);
#3772=AXIS2_PLACEMENT_3D('',#9287,#4469,#4470);
#3773=AXIS2_PLACEMENT_3D('',#9288,#4471,#4472);
#3774=AXIS2_PLACEMENT_3D('',#9290,#4473,#4474);
#3775=AXIS2_PLACEMENT_3D('',#9293,#4476,#4477);
#3776=AXIS2_PLACEMENT_3D('',#9294,#4478,#4479);
#3777=AXIS2_PLACEMENT_3D('',#9297,#4480,#4481);
#3778=AXIS2_PLACEMENT_3D('',#9301,#4483,#4484);
#3779=AXIS2_PLACEMENT_3D('',#9303,#4486,#4487);
#3780=AXIS2_PLACEMENT_3D('',#9320,#4496,#4497);
#3781=AXIS2_PLACEMENT_3D('',#9326,#4501,#4502);
#3782=AXIS2_PLACEMENT_3D('',#9340,#4510,#4511);
#3783=AXIS2_PLACEMENT_3D('',#9343,#4514,#4515);
#3784=AXIS2_PLACEMENT_3D('',#9346,#4518,#4519);
#3785=AXIS2_PLACEMENT_3D('',#9347,#4520,#4521);
#3786=AXIS2_PLACEMENT_3D('',#9349,#4523,#4524);
#3787=AXIS2_PLACEMENT_3D('',#9351,#4526,#4527);
#3788=AXIS2_PLACEMENT_3D('',#9357,#4531,#4532);
#3789=AXIS2_PLACEMENT_3D('',#9363,#4536,#4537);
#3790=AXIS2_PLACEMENT_3D('',#9364,#4538,#4539);
#3791=AXIS2_PLACEMENT_3D('',#9365,#4540,#4541);
#3792=AXIS2_PLACEMENT_3D('',#9366,#4542,#4543);
#3793=AXIS2_PLACEMENT_3D('',#9367,#4544,#4545);
#3794=AXIS2_PLACEMENT_3D('',#9368,#4546,#4547);
#3795=AXIS2_PLACEMENT_3D('',#11319,#4548,#4549);
#3796=AXIS2_PLACEMENT_3D('',#11562,#4550,#4551);
#3797=AXIS2_PLACEMENT_3D('',#11563,#4552,#4553);
#3798=AXIS2_PLACEMENT_3D('',#11565,#4554,#4555);
#3799=AXIS2_PLACEMENT_3D('',#13274,#4557,#4558);
#3800=AXIS2_PLACEMENT_3D('',#13275,#4559,#4560);
#3801=AXIS2_PLACEMENT_3D('',#13276,#4561,#4562);
#3802=AXIS2_PLACEMENT_3D('',#13277,#4563,#4564);
#3803=AXIS2_PLACEMENT_3D('',#13278,#4565,#4566);
#3804=AXIS2_PLACEMENT_3D('',#13280,#4567,#4568);
#3805=AXIS2_PLACEMENT_3D('',#13284,#4570,#4571);
#3806=AXIS2_PLACEMENT_3D('',#13285,#4572,#4573);
#3807=AXIS2_PLACEMENT_3D('',#13286,#4574,#4575);
#3808=AXIS2_PLACEMENT_3D('',#13289,#4576,#4577);
#3809=AXIS2_PLACEMENT_3D('',#13291,#4579,#4580);
#3810=AXIS2_PLACEMENT_3D('',#13292,#4581,#4582);
#3811=AXIS2_PLACEMENT_3D('',#13294,#4583,#4584);
#3812=AXIS2_PLACEMENT_3D('',#13297,#4586,#4587);
#3813=AXIS2_PLACEMENT_3D('',#13298,#4588,#4589);
#3814=AXIS2_PLACEMENT_3D('',#13301,#4590,#4591);
#3815=AXIS2_PLACEMENT_3D('',#13391,#4593,#4594);
#3816=AXIS2_PLACEMENT_3D('',#13392,#4595,#4596);
#3817=AXIS2_PLACEMENT_3D('',#13394,#4597,#4598);
#3818=AXIS2_PLACEMENT_3D('',#13395,#4599,#4600);
#3819=AXIS2_PLACEMENT_3D('',#13396,#4601,#4602);
#3820=AXIS2_PLACEMENT_3D('',#13398,#4604,#4605);
#3821=AXIS2_PLACEMENT_3D('',#13449,#4608,#4609);
#3822=AXIS2_PLACEMENT_3D('',#13497,#4611,#4612);
#3823=AXIS2_PLACEMENT_3D('',#13545,#4614,#4615);
#3824=AXIS2_PLACEMENT_3D('',#13593,#4617,#4618);
#3825=AXIS2_PLACEMENT_3D('',#13641,#4620,#4621);
#3826=AXIS2_PLACEMENT_3D('',#13686,#4622,#4623);
#3827=AXIS2_PLACEMENT_3D('',#13687,#4624,#4625);
#3828=AXIS2_PLACEMENT_3D('',#13688,#4626,#4627);
#3829=AXIS2_PLACEMENT_3D('',#13689,#4628,#4629);
#3830=AXIS2_PLACEMENT_3D('',#13690,#4630,#4631);
#3831=AXIS2_PLACEMENT_3D('',#13691,#4632,#4633);
#3832=AXIS2_PLACEMENT_3D('',#13692,#4634,#4635);
#3833=AXIS2_PLACEMENT_3D('',#13693,#4636,#4637);
#3834=AXIS2_PLACEMENT_3D('',#13694,#4638,#4639);
#3835=AXIS2_PLACEMENT_3D('',#13695,#4640,#4641);
#3836=AXIS2_PLACEMENT_3D('',#13696,#4642,#4643);
#3837=AXIS2_PLACEMENT_3D('',#13697,#4644,#4645);
#3838=AXIS2_PLACEMENT_3D('',#13698,#4646,#4647);
#3839=AXIS2_PLACEMENT_3D('',#13699,#4648,#4649);
#3840=AXIS2_PLACEMENT_3D('',#14030,#4650,#4651);
#3841=AXIS2_PLACEMENT_3D('',#14031,#4652,#4653);
#3842=AXIS2_PLACEMENT_3D('',#14033,#4654,#4655);
#3843=AXIS2_PLACEMENT_3D('',#14036,#4657,#4658);
#3844=AXIS2_PLACEMENT_3D('',#14037,#4659,#4660);
#3845=AXIS2_PLACEMENT_3D('',#14039,#4661,#4662);
#3846=AXIS2_PLACEMENT_3D('',#14042,#4664,#4665);
#3847=AXIS2_PLACEMENT_3D('',#14043,#4666,#4667);
#3848=AXIS2_PLACEMENT_3D('',#14045,#4668,#4669);
#3849=AXIS2_PLACEMENT_3D('',#14048,#4671,#4672);
#3850=AXIS2_PLACEMENT_3D('',#14049,#4673,#4674);
#3851=AXIS2_PLACEMENT_3D('',#14050,#4675,#4676);
#3852=AXIS2_PLACEMENT_3D('',#14051,#4677,#4678);
#3853=AXIS2_PLACEMENT_3D('',#14052,#4679,#4680);
#3854=AXIS2_PLACEMENT_3D('',#14053,#4681,#4682);
#3855=AXIS2_PLACEMENT_3D('',#14054,#4683,#4684);
#3856=AXIS2_PLACEMENT_3D('',#14055,#4685,#4686);
#3857=AXIS2_PLACEMENT_3D('',#14056,#4687,#4688);
#3858=AXIS2_PLACEMENT_3D('',#14057,#4689,#4690);
#3859=AXIS2_PLACEMENT_3D('',#14058,#4691,#4692);
#3860=AXIS2_PLACEMENT_3D('',#14059,#4693,#4694);
#3861=AXIS2_PLACEMENT_3D('',#14060,#4695,#4696);
#3862=AXIS2_PLACEMENT_3D('',#14061,#4697,#4698);
#3863=AXIS2_PLACEMENT_3D('',#14062,#4699,#4700);
#3864=DIRECTION('axis',(0.,0.,1.));
#3865=DIRECTION('refdir',(1.,0.,0.));
#3866=DIRECTION('axis',(0.,0.,1.));
#3867=DIRECTION('refdir',(1.,0.,0.));
#3868=DIRECTION('center_axis',(0.,-1.,0.));
#3869=DIRECTION('ref_axis',(0.,0.,-1.));
#3870=DIRECTION('center_axis',(0.,1.,0.));
#3871=DIRECTION('ref_axis',(0.,0.,1.));
#3872=DIRECTION('',(0.,-1.,0.));
#3873=DIRECTION('center_axis',(0.,1.,0.));
#3874=DIRECTION('ref_axis',(0.,0.,1.));
#3875=DIRECTION('center_axis',(0.,-1.,0.));
#3876=DIRECTION('ref_axis',(0.,0.,-1.));
#3877=DIRECTION('center_axis',(0.,1.,0.));
#3878=DIRECTION('ref_axis',(1.,0.,0.));
#3879=DIRECTION('',(0.,1.,0.));
#3880=DIRECTION('center_axis',(0.,1.,0.));
#3881=DIRECTION('ref_axis',(1.,0.,0.));
#3882=DIRECTION('',(0.,-1.,0.));
#3883=DIRECTION('center_axis',(0.,1.,0.));
#3884=DIRECTION('ref_axis',(0.,0.,1.));
#3885=DIRECTION('',(1.,0.,0.));
#3886=DIRECTION('',(0.,0.,1.));
#3887=DIRECTION('',(-1.,0.,0.));
#3888=DIRECTION('center_axis',(0.,1.,0.));
#3889=DIRECTION('ref_axis',(1.,0.,0.));
#3890=DIRECTION('',(-1.,0.,2.89120579329468E-16));
#3891=DIRECTION('',(0.,0.,-1.));
#3892=DIRECTION('',(1.,0.,-2.89120579329468E-16));
#3893=DIRECTION('center_axis',(0.,-1.,0.));
#3894=DIRECTION('ref_axis',(-1.22464679914735E-16,0.,1.));
#3895=DIRECTION('',(0.,1.,0.));
#3896=DIRECTION('center_axis',(0.,1.,0.));
#3897=DIRECTION('ref_axis',(1.,0.,0.));
#3898=DIRECTION('',(0.,-1.,0.));
#3899=DIRECTION('center_axis',(0.,1.,0.));
#3900=DIRECTION('ref_axis',(0.,0.,1.));
#3901=DIRECTION('',(1.,0.,0.));
#3902=DIRECTION('',(0.,0.,1.));
#3903=DIRECTION('',(-1.,0.,0.));
#3904=DIRECTION('',(-1.,0.,2.89120579329468E-16));
#3905=DIRECTION('',(0.,0.,-1.));
#3906=DIRECTION('',(1.,0.,-2.89120579329468E-16));
#3907=DIRECTION('center_axis',(-1.,0.,0.));
#3908=DIRECTION('ref_axis',(0.,0.,1.));
#3909=DIRECTION('',(0.,-1.,0.));
#3910=DIRECTION('',(0.,0.,-1.));
#3911=DIRECTION('',(0.,-1.,0.));
#3912=DIRECTION('center_axis',(2.89120579329468E-16,0.,1.));
#3913=DIRECTION('ref_axis',(1.,0.,-2.89120579329468E-16));
#3914=DIRECTION('',(0.,-1.,0.));
#3915=DIRECTION('',(-1.,0.,2.89120579329468E-16));
#3916=DIRECTION('center_axis',(1.,0.,0.));
#3917=DIRECTION('ref_axis',(0.,0.,-1.));
#3918=DIRECTION('',(0.,-1.,0.));
#3919=DIRECTION('',(0.,0.,1.));
#3920=DIRECTION('center_axis',(-2.89120579329468E-16,0.,-1.));
#3921=DIRECTION('ref_axis',(-1.,0.,2.89120579329468E-16));
#3922=DIRECTION('',(1.,0.,-2.89120579329468E-16));
#3923=DIRECTION('center_axis',(0.,1.,0.));
#3924=DIRECTION('ref_axis',(0.,0.,1.));
#3925=DIRECTION('center_axis',(-1.,0.,0.));
#3926=DIRECTION('ref_axis',(0.,0.,1.));
#3927=DIRECTION('',(0.,-1.,0.));
#3928=DIRECTION('',(0.,0.,-1.));
#3929=DIRECTION('',(0.,-1.,0.));
#3930=DIRECTION('center_axis',(0.,0.,1.));
#3931=DIRECTION('ref_axis',(1.,0.,0.));
#3932=DIRECTION('',(0.,-1.,0.));
#3933=DIRECTION('',(-1.,0.,0.));
#3934=DIRECTION('center_axis',(1.,0.,0.));
#3935=DIRECTION('ref_axis',(0.,0.,-1.));
#3936=DIRECTION('',(0.,-1.,0.));
#3937=DIRECTION('',(0.,0.,1.));
#3938=DIRECTION('center_axis',(0.,0.,-1.));
#3939=DIRECTION('ref_axis',(-1.,0.,0.));
#3940=DIRECTION('',(1.,0.,0.));
#3941=DIRECTION('center_axis',(0.,-1.,0.));
#3942=DIRECTION('ref_axis',(0.,0.,-1.));
#3943=DIRECTION('axis',(0.,0.,1.));
#3944=DIRECTION('refdir',(1.,0.,0.));
#3945=DIRECTION('center_axis',(0.,0.,1.));
#3946=DIRECTION('ref_axis',(1.,0.,0.));
#3947=DIRECTION('center_axis',(0.,0.,-1.));
#3948=DIRECTION('ref_axis',(-1.,0.,0.));
#3949=DIRECTION('',(0.,0.,1.));
#3950=DIRECTION('center_axis',(0.,0.,-1.));
#3951=DIRECTION('ref_axis',(-1.,0.,0.));
#3952=DIRECTION('center_axis',(0.,1.,0.));
#3953=DIRECTION('ref_axis',(0.,0.,1.));
#3954=DIRECTION('center_axis',(0.,1.,0.));
#3955=DIRECTION('ref_axis',(0.,0.,1.));
#3956=DIRECTION('',(0.,1.,0.));
#3957=DIRECTION('center_axis',(0.,-1.,0.));
#3958=DIRECTION('ref_axis',(0.,0.,-1.));
#3959=DIRECTION('center_axis',(0.,1.,0.));
#3960=DIRECTION('ref_axis',(0.,0.,1.));
#3961=DIRECTION('center_axis',(0.,1.,0.));
#3962=DIRECTION('ref_axis',(0.,0.,1.));
#3963=DIRECTION('',(0.,1.,0.));
#3964=DIRECTION('center_axis',(0.,1.,0.));
#3965=DIRECTION('ref_axis',(0.,0.,1.));
#3966=DIRECTION('center_axis',(0.,1.,0.));
#3967=DIRECTION('ref_axis',(0.,0.,1.));
#3968=DIRECTION('center_axis',(0.,1.,0.));
#3969=DIRECTION('ref_axis',(0.,0.,1.));
#3970=DIRECTION('',(0.,-1.,0.));
#3971=DIRECTION('center_axis',(0.,1.,0.));
#3972=DIRECTION('ref_axis',(0.,0.,1.));
#3973=DIRECTION('',(0.,1.,0.));
#3974=DIRECTION('center_axis',(0.,1.,0.));
#3975=DIRECTION('ref_axis',(0.,0.,1.));
#3976=DIRECTION('center_axis',(0.,1.,0.));
#3977=DIRECTION('ref_axis',(0.,0.,1.));
#3978=DIRECTION('',(0.,-1.,0.));
#3979=DIRECTION('center_axis',(0.,1.,0.));
#3980=DIRECTION('ref_axis',(0.,0.,1.));
#3981=DIRECTION('',(0.,1.,0.));
#3982=DIRECTION('center_axis',(1.,0.,0.));
#3983=DIRECTION('ref_axis',(0.,0.,-1.));
#3984=DIRECTION('',(0.,1.,0.));
#3985=DIRECTION('',(0.,0.,-1.));
#3986=DIRECTION('',(0.,1.,0.));
#3987=DIRECTION('',(0.,0.,1.));
#3988=DIRECTION('',(0.,-1.,0.));
#3989=DIRECTION('',(0.,0.,1.));
#3990=DIRECTION('',(0.,-1.,0.));
#3991=DIRECTION('',(0.,0.,1.));
#3992=DIRECTION('',(0.,-1.,0.));
#3993=DIRECTION('',(0.,0.,1.));
#3994=DIRECTION('',(0.,-1.,0.));
#3995=DIRECTION('',(0.,0.,1.));
#3996=DIRECTION('center_axis',(-2.16840434497101E-16,0.,-1.));
#3997=DIRECTION('ref_axis',(-1.,0.,2.16840434497101E-16));
#3998=DIRECTION('',(1.,0.,0.));
#3999=DIRECTION('',(1.,0.,-2.16840434497101E-16));
#4000=DIRECTION('',(0.,-1.,0.));
#4001=DIRECTION('center_axis',(0.,1.,0.));
#4002=DIRECTION('ref_axis',(0.,0.,1.));
#4003=DIRECTION('',(1.,0.,0.));
#4004=DIRECTION('',(0.,0.,-1.));
#4005=DIRECTION('',(1.,0.,0.));
#4006=DIRECTION('center_axis',(0.,1.,0.));
#4007=DIRECTION('ref_axis',(0.,0.,1.));
#4008=DIRECTION('',(1.,0.,0.));
#4009=DIRECTION('',(0.,0.,-1.));
#4010=DIRECTION('',(-1.,0.,0.));
#4011=DIRECTION('',(0.,0.,1.));
#4012=DIRECTION('',(1.,0.,0.));
#4013=DIRECTION('',(0.,0.,-1.));
#4014=DIRECTION('',(1.,0.,0.));
#4015=DIRECTION('center_axis',(0.,0.,-1.));
#4016=DIRECTION('ref_axis',(-1.,0.,0.));
#4017=DIRECTION('',(1.,0.,0.));
#4018=DIRECTION('',(0.,-1.,0.));
#4019=DIRECTION('center_axis',(0.,0.,-1.));
#4020=DIRECTION('ref_axis',(-1.,0.,0.));
#4021=DIRECTION('',(0.,1.,0.));
#4022=DIRECTION('',(1.,0.,0.));
#4023=DIRECTION('',(0.,-1.,0.));
#4024=DIRECTION('center_axis',(1.,0.,0.));
#4025=DIRECTION('ref_axis',(0.,0.,-1.));
#4026=DIRECTION('',(0.,0.,1.));
#4027=DIRECTION('',(0.,1.,0.));
#4028=DIRECTION('',(0.,0.,-1.));
#4029=DIRECTION('',(0.,0.,1.));
#4030=DIRECTION('',(0.,-1.,0.));
#4031=DIRECTION('',(0.,0.,-1.));
#4032=DIRECTION('',(0.,-1.,0.));
#4033=DIRECTION('center_axis',(-1.,0.,0.));
#4034=DIRECTION('ref_axis',(0.,0.,1.));
#4035=DIRECTION('',(0.,-1.,0.));
#4036=DIRECTION('',(0.,0.,-1.));
#4037=DIRECTION('',(0.,1.,0.));
#4038=DIRECTION('',(0.,0.,-1.));
#4039=DIRECTION('',(0.,1.,0.));
#4040=DIRECTION('',(0.,0.,-1.));
#4041=DIRECTION('',(0.,-1.,0.));
#4042=DIRECTION('',(0.,0.,-1.));
#4043=DIRECTION('center_axis',(0.,0.,-1.));
#4044=DIRECTION('ref_axis',(-1.,0.,0.));
#4045=DIRECTION('',(1.,0.,0.));
#4046=DIRECTION('',(1.,0.,0.));
#4047=DIRECTION('center_axis',(0.,0.,-1.));
#4048=DIRECTION('ref_axis',(-1.,0.,0.));
#4049=DIRECTION('',(1.,0.,0.));
#4050=DIRECTION('',(1.,0.,0.));
#4051=DIRECTION('',(0.,1.,0.));
#4052=DIRECTION('center_axis',(0.,0.,-1.));
#4053=DIRECTION('ref_axis',(-1.,0.,0.));
#4054=DIRECTION('',(1.,0.,0.));
#4055=DIRECTION('',(1.,0.,0.));
#4056=DIRECTION('center_axis',(0.,0.,-1.));
#4057=DIRECTION('ref_axis',(-1.,0.,0.));
#4058=DIRECTION('',(1.,0.,0.));
#4059=DIRECTION('',(1.,0.,0.));
#4060=DIRECTION('',(0.,-1.,0.));
#4061=DIRECTION('center_axis',(0.,-1.,0.));
#4062=DIRECTION('ref_axis',(-1.,0.,0.));
#4063=DIRECTION('center_axis',(0.,1.,0.));
#4064=DIRECTION('ref_axis',(0.,0.,1.));
#4065=DIRECTION('center_axis',(-1.,0.,0.));
#4066=DIRECTION('ref_axis',(0.,0.,1.));
#4067=DIRECTION('',(0.,-1.,0.));
#4068=DIRECTION('',(0.,-1.,0.));
#4069=DIRECTION('',(0.,0.,-1.));
#4070=DIRECTION('center_axis',(0.,-1.,0.));
#4071=DIRECTION('ref_axis',(-1.,0.,0.));
#4072=DIRECTION('',(1.,0.,0.));
#4073=DIRECTION('',(-1.,0.,0.));
#4074=DIRECTION('center_axis',(0.,1.,0.));
#4075=DIRECTION('ref_axis',(0.,0.,1.));
#4076=DIRECTION('',(-1.,0.,2.16840434497101E-16));
#4077=DIRECTION('center_axis',(0.,1.,0.));
#4078=DIRECTION('ref_axis',(1.22464679914735E-16,0.,-1.));
#4079=DIRECTION('center_axis',(2.16840434497101E-16,0.,1.));
#4080=DIRECTION('ref_axis',(1.,0.,-2.16840434497101E-16));
#4081=DIRECTION('',(1.,0.,0.));
#4082=DIRECTION('center_axis',(0.,0.,-1.));
#4083=DIRECTION('ref_axis',(-1.,0.,0.));
#4084=DIRECTION('center_axis',(0.,0.,1.));
#4085=DIRECTION('ref_axis',(1.,0.,0.));
#4086=DIRECTION('center_axis',(0.,0.,-1.));
#4087=DIRECTION('ref_axis',(-1.,0.,0.));
#4088=DIRECTION('',(0.,-1.,0.));
#4089=DIRECTION('center_axis',(0.,0.,1.));
#4090=DIRECTION('ref_axis',(-1.,0.,0.));
#4091=DIRECTION('',(1.,0.,0.));
#4092=DIRECTION('',(1.,0.,0.));
#4093=DIRECTION('',(0.984807753012208,0.173648177666931,0.));
#4094=DIRECTION('',(0.173648177666933,-0.984807753012208,0.));
#4095=DIRECTION('',(0.984807753012208,0.173648177666931,0.));
#4096=DIRECTION('',(1.,0.,0.));
#4097=DIRECTION('center_axis',(0.,0.,-1.));
#4098=DIRECTION('ref_axis',(-1.,0.,0.));
#4099=DIRECTION('center_axis',(0.,0.,-1.));
#4100=DIRECTION('ref_axis',(-1.,0.,0.));
#4101=DIRECTION('',(0.,-1.,0.));
#4102=DIRECTION('',(1.,0.,0.));
#4103=DIRECTION('',(0.,-1.,0.));
#4104=DIRECTION('',(0.984807753012208,0.173648177666931,0.));
#4105=DIRECTION('',(0.173648177666933,-0.984807753012208,0.));
#4106=DIRECTION('',(0.984807753012208,0.173648177666931,0.));
#4107=DIRECTION('',(1.,0.,0.));
#4108=DIRECTION('',(1.,0.,0.));
#4109=DIRECTION('center_axis',(0.,1.,0.));
#4110=DIRECTION('ref_axis',(0.,0.,1.));
#4111=DIRECTION('',(0.,0.,1.));
#4112=DIRECTION('center_axis',(0.,1.,0.));
#4113=DIRECTION('ref_axis',(0.,0.,1.));
#4114=DIRECTION('center_axis',(0.,1.,0.));
#4115=DIRECTION('ref_axis',(0.,0.,1.));
#4116=DIRECTION('',(0.,0.,-1.));
#4117=DIRECTION('center_axis',(-0.173648177666931,0.984807753012208,0.));
#4118=DIRECTION('ref_axis',(-0.984807753012208,-0.173648177666931,0.));
#4119=DIRECTION('',(0.,0.,-1.));
#4120=DIRECTION('center_axis',(0.984807753012208,0.173648177666933,0.));
#4121=DIRECTION('ref_axis',(-0.173648177666933,0.984807753012208,0.));
#4122=DIRECTION('',(0.,0.,-1.));
#4123=DIRECTION('center_axis',(-0.173648177666931,0.984807753012208,0.));
#4124=DIRECTION('ref_axis',(-0.984807753012208,-0.173648177666931,0.));
#4125=DIRECTION('center_axis',(0.,1.,0.));
#4126=DIRECTION('ref_axis',(1.22464679914735E-16,0.,-1.));
#4127=DIRECTION('center_axis',(0.,-1.,0.));
#4128=DIRECTION('ref_axis',(0.,0.,-1.));
#4129=DIRECTION('center_axis',(0.,-1.,0.));
#4130=DIRECTION('ref_axis',(0.,0.,-1.));
#4131=DIRECTION('center_axis',(-1.,0.,0.));
#4132=DIRECTION('ref_axis',(0.,0.,1.));
#4133=DIRECTION('',(0.,0.,1.));
#4134=DIRECTION('center_axis',(0.,0.,1.));
#4135=DIRECTION('ref_axis',(1.,0.,0.));
#4136=DIRECTION('axis',(0.,0.,1.));
#4137=DIRECTION('refdir',(1.,0.,0.));
#4138=DIRECTION('center_axis',(0.,-1.,0.));
#4139=DIRECTION('ref_axis',(1.,0.,4.82166445138931E-17));
#4140=DIRECTION('',(0.,1.,0.));
#4141=DIRECTION('',(0.,1.,0.));
#4142=DIRECTION('center_axis',(0.,-1.,0.));
#4143=DIRECTION('ref_axis',(1.,0.,4.82166445138931E-17));
#4144=DIRECTION('',(0.,1.,0.));
#4145=DIRECTION('center_axis',(0.,-1.,0.));
#4146=DIRECTION('ref_axis',(1.,0.,4.82166445138931E-17));
#4147=DIRECTION('',(0.,1.,0.));
#4148=DIRECTION('center_axis',(0.,-1.,0.));
#4149=DIRECTION('ref_axis',(1.,0.,4.82166445138931E-17));
#4150=DIRECTION('',(0.,1.,0.));
#4151=DIRECTION('center_axis',(0.,-1.,0.));
#4152=DIRECTION('ref_axis',(1.,0.,4.82166445138931E-17));
#4153=DIRECTION('',(0.,1.,0.));
#4154=DIRECTION('center_axis',(0.,-1.,0.));
#4155=DIRECTION('ref_axis',(1.,0.,4.82166445138931E-17));
#4156=DIRECTION('',(0.,1.,0.));
#4157=DIRECTION('center_axis',(0.,-1.,0.));
#4158=DIRECTION('ref_axis',(1.,0.,4.82166445138931E-17));
#4159=DIRECTION('',(0.,1.,0.));
#4160=DIRECTION('center_axis',(0.,-1.,0.));
#4161=DIRECTION('ref_axis',(1.,0.,4.82166445138931E-17));
#4162=DIRECTION('',(0.,1.,0.));
#4163=DIRECTION('center_axis',(0.,-1.,0.));
#4164=DIRECTION('ref_axis',(1.,0.,4.82166445138931E-17));
#4165=DIRECTION('',(0.,1.,0.));
#4166=DIRECTION('center_axis',(0.,-1.,0.));
#4167=DIRECTION('ref_axis',(1.,0.,4.82166445138931E-17));
#4168=DIRECTION('',(0.,1.,0.));
#4169=DIRECTION('center_axis',(0.,-1.,0.));
#4170=DIRECTION('ref_axis',(1.,0.,4.82166445138931E-17));
#4171=DIRECTION('',(0.,1.,0.));
#4172=DIRECTION('center_axis',(0.,-1.,0.));
#4173=DIRECTION('ref_axis',(1.,0.,4.82166445138931E-17));
#4174=DIRECTION('',(0.,1.,0.));
#4175=DIRECTION('center_axis',(0.,-1.,0.));
#4176=DIRECTION('ref_axis',(1.,0.,4.82166445138931E-17));
#4177=DIRECTION('',(0.,1.,0.));
#4178=DIRECTION('center_axis',(0.,-1.,0.));
#4179=DIRECTION('ref_axis',(1.,0.,4.82166445138931E-17));
#4180=DIRECTION('',(0.,1.,0.));
#4181=DIRECTION('center_axis',(0.,-1.,0.));
#4182=DIRECTION('ref_axis',(1.,0.,4.82166445138931E-17));
#4183=DIRECTION('',(0.,1.,0.));
#4184=DIRECTION('center_axis',(0.,-1.,0.));
#4185=DIRECTION('ref_axis',(1.,0.,4.82166445138931E-17));
#4186=DIRECTION('',(0.,1.,0.));
#4187=DIRECTION('center_axis',(0.,-1.,0.));
#4188=DIRECTION('ref_axis',(1.,0.,4.82166445138931E-17));
#4189=DIRECTION('',(0.,1.,0.));
#4190=DIRECTION('center_axis',(0.,-1.,0.));
#4191=DIRECTION('ref_axis',(1.,0.,4.82166445138931E-17));
#4192=DIRECTION('',(0.,1.,0.));
#4193=DIRECTION('center_axis',(0.,-1.,0.));
#4194=DIRECTION('ref_axis',(1.,0.,4.82166445138931E-17));
#4195=DIRECTION('',(0.,1.,0.));
#4196=DIRECTION('center_axis',(0.,-1.,0.));
#4197=DIRECTION('ref_axis',(1.,0.,4.82166445138931E-17));
#4198=DIRECTION('',(0.,1.,0.));
#4199=DIRECTION('center_axis',(0.,-1.,0.));
#4200=DIRECTION('ref_axis',(1.,0.,4.82166445138931E-17));
#4201=DIRECTION('',(0.,1.,0.));
#4202=DIRECTION('center_axis',(0.,-1.,0.));
#4203=DIRECTION('ref_axis',(1.,0.,4.82166445138931E-17));
#4204=DIRECTION('',(0.,1.,0.));
#4205=DIRECTION('center_axis',(0.,-1.,0.));
#4206=DIRECTION('ref_axis',(1.,0.,4.82166445138931E-17));
#4207=DIRECTION('',(0.,1.,0.));
#4208=DIRECTION('center_axis',(0.,-1.,0.));
#4209=DIRECTION('ref_axis',(1.,0.,4.82166445138931E-17));
#4210=DIRECTION('',(0.,1.,0.));
#4211=DIRECTION('center_axis',(0.,-1.,0.));
#4212=DIRECTION('ref_axis',(1.,0.,4.82166445138931E-17));
#4213=DIRECTION('',(0.,1.,0.));
#4214=DIRECTION('center_axis',(0.,-1.,0.));
#4215=DIRECTION('ref_axis',(1.,0.,4.82166445138931E-17));
#4216=DIRECTION('',(0.,1.,0.));
#4217=DIRECTION('center_axis',(0.,-1.,0.));
#4218=DIRECTION('ref_axis',(1.,0.,4.82166445138931E-17));
#4219=DIRECTION('',(0.,1.,0.));
#4220=DIRECTION('center_axis',(0.,1.,0.));
#4221=DIRECTION('ref_axis',(0.,0.,1.));
#4222=DIRECTION('',(0.,-1.,0.));
#4223=DIRECTION('center_axis',(-2.67523620391605E-16,-1.,0.));
#4224=DIRECTION('ref_axis',(1.,-2.67523620391605E-16,0.));
#4225=DIRECTION('center_axis',(0.,1.,0.));
#4226=DIRECTION('ref_axis',(0.,0.,1.));
#4227=DIRECTION('',(0.,-1.,0.));
#4228=DIRECTION('center_axis',(-2.67523620391605E-16,-1.,0.));
#4229=DIRECTION('ref_axis',(1.,-2.67523620391605E-16,0.));
#4230=DIRECTION('',(0.,1.,0.));
#4231=DIRECTION('center_axis',(0.,1.,0.));
#4232=DIRECTION('ref_axis',(0.,0.,1.));
#4233=DIRECTION('',(0.,-1.,0.));
#4234=DIRECTION('center_axis',(0.,1.,0.));
#4235=DIRECTION('ref_axis',(0.,0.,1.));
#4236=DIRECTION('',(0.,-1.,0.));
#4237=DIRECTION('center_axis',(0.,1.,0.));
#4238=DIRECTION('ref_axis',(0.,0.,1.));
#4239=DIRECTION('',(0.,-1.,0.));
#4240=DIRECTION('center_axis',(0.,1.,0.));
#4241=DIRECTION('ref_axis',(0.,0.,1.));
#4242=DIRECTION('',(0.,-1.,0.));
#4243=DIRECTION('center_axis',(0.,1.,0.));
#4244=DIRECTION('ref_axis',(0.,0.,1.));
#4245=DIRECTION('',(0.,-1.,0.));
#4246=DIRECTION('center_axis',(0.,1.,0.));
#4247=DIRECTION('ref_axis',(0.,0.,1.));
#4248=DIRECTION('',(0.,-1.,0.));
#4249=DIRECTION('center_axis',(0.,1.,0.));
#4250=DIRECTION('ref_axis',(0.,0.,1.));
#4251=DIRECTION('',(0.,-1.,0.));
#4252=DIRECTION('center_axis',(0.,1.,0.));
#4253=DIRECTION('ref_axis',(0.,0.,1.));
#4254=DIRECTION('',(0.,-1.,0.));
#4255=DIRECTION('center_axis',(0.,1.,0.));
#4256=DIRECTION('ref_axis',(0.,0.,1.));
#4257=DIRECTION('',(0.,-1.,0.));
#4258=DIRECTION('center_axis',(0.,1.,0.));
#4259=DIRECTION('ref_axis',(0.,0.,1.));
#4260=DIRECTION('',(0.,-1.,0.));
#4261=DIRECTION('center_axis',(0.,1.,0.));
#4262=DIRECTION('ref_axis',(0.,0.,1.));
#4263=DIRECTION('',(0.,-1.,0.));
#4264=DIRECTION('center_axis',(0.,1.,0.));
#4265=DIRECTION('ref_axis',(0.,0.,1.));
#4266=DIRECTION('',(0.,-1.,0.));
#4267=DIRECTION('center_axis',(0.,1.,0.));
#4268=DIRECTION('ref_axis',(0.,0.,1.));
#4269=DIRECTION('',(0.,-1.,0.));
#4270=DIRECTION('center_axis',(0.,1.,0.));
#4271=DIRECTION('ref_axis',(0.,0.,1.));
#4272=DIRECTION('',(0.,-1.,0.));
#4273=DIRECTION('center_axis',(0.,1.,0.));
#4274=DIRECTION('ref_axis',(0.,0.,1.));
#4275=DIRECTION('',(0.,-1.,0.));
#4276=DIRECTION('center_axis',(0.,1.,0.));
#4277=DIRECTION('ref_axis',(0.,0.,1.));
#4278=DIRECTION('',(0.,-1.,0.));
#4279=DIRECTION('center_axis',(0.,1.,0.));
#4280=DIRECTION('ref_axis',(0.,0.,1.));
#4281=DIRECTION('',(0.,-1.,0.));
#4282=DIRECTION('center_axis',(0.,1.,0.));
#4283=DIRECTION('ref_axis',(0.,0.,1.));
#4284=DIRECTION('',(0.,-1.,0.));
#4285=DIRECTION('center_axis',(0.,1.,0.));
#4286=DIRECTION('ref_axis',(0.,0.,1.));
#4287=DIRECTION('',(0.,-1.,0.));
#4288=DIRECTION('center_axis',(0.,1.,0.));
#4289=DIRECTION('ref_axis',(0.,0.,1.));
#4290=DIRECTION('',(0.,-1.,0.));
#4291=DIRECTION('center_axis',(0.,1.,0.));
#4292=DIRECTION('ref_axis',(0.,0.,1.));
#4293=DIRECTION('',(0.,-1.,0.));
#4294=DIRECTION('center_axis',(0.,1.,0.));
#4295=DIRECTION('ref_axis',(0.,0.,1.));
#4296=DIRECTION('',(0.,-1.,0.));
#4297=DIRECTION('center_axis',(0.,1.,0.));
#4298=DIRECTION('ref_axis',(0.,0.,1.));
#4299=DIRECTION('',(0.,-1.,0.));
#4300=DIRECTION('center_axis',(0.,1.,0.));
#4301=DIRECTION('ref_axis',(0.,0.,1.));
#4302=DIRECTION('',(0.,-1.,0.));
#4303=DIRECTION('center_axis',(0.,1.,0.));
#4304=DIRECTION('ref_axis',(0.,0.,1.));
#4305=DIRECTION('center_axis',(0.,-1.,0.));
#4306=DIRECTION('ref_axis',(0.,0.,-1.));
#4307=DIRECTION('',(0.,-1.,0.));
#4308=DIRECTION('',(0.,-1.,0.));
#4309=DIRECTION('',(0.,-1.,0.));
#4310=DIRECTION('center_axis',(0.,0.,1.));
#4311=DIRECTION('ref_axis',(1.,0.,0.));
#4312=DIRECTION('center_axis',(2.67523620391605E-16,1.,0.));
#4313=DIRECTION('ref_axis',(-1.,2.67523620391605E-16,0.));
#4314=DIRECTION('center_axis',(0.,0.,-1.));
#4315=DIRECTION('ref_axis',(1.,0.,0.));
#4316=DIRECTION('center_axis',(-2.67523620391605E-16,-1.,0.));
#4317=DIRECTION('ref_axis',(1.,-2.67523620391605E-16,0.));
#4318=DIRECTION('center_axis',(-2.67523620391605E-16,-1.,0.));
#4319=DIRECTION('ref_axis',(1.,-2.67523620391605E-16,0.));
#4320=DIRECTION('center_axis',(0.,1.,0.));
#4321=DIRECTION('ref_axis',(0.,0.,1.));
#4322=DIRECTION('center_axis',(0.,1.,0.));
#4323=DIRECTION('ref_axis',(0.,0.,1.));
#4324=DIRECTION('center_axis',(0.,-1.,0.));
#4325=DIRECTION('ref_axis',(0.,0.,-1.));
#4326=DIRECTION('',(0.,-1.,0.));
#4327=DIRECTION('center_axis',(0.,-1.,0.));
#4328=DIRECTION('ref_axis',(0.,0.,-1.));
#4329=DIRECTION('center_axis',(0.,1.,0.));
#4330=DIRECTION('ref_axis',(0.,0.,1.));
#4331=DIRECTION('',(0.,-1.,0.));
#4332=DIRECTION('center_axis',(0.,-1.,0.));
#4333=DIRECTION('ref_axis',(0.,0.,-1.));
#4334=DIRECTION('center_axis',(2.67523620391605E-16,1.,0.));
#4335=DIRECTION('ref_axis',(-1.,2.67523620391605E-16,0.));
#4336=DIRECTION('center_axis',(0.,-1.,0.));
#4337=DIRECTION('ref_axis',(0.,0.,-1.));
#4338=DIRECTION('center_axis',(0.,-1.,0.));
#4339=DIRECTION('ref_axis',(0.,0.,-1.));
#4340=DIRECTION('center_axis',(-2.67523620391605E-16,-1.,0.));
#4341=DIRECTION('ref_axis',(1.,-2.67523620391605E-16,0.));
#4342=DIRECTION('center_axis',(0.,0.,1.));
#4343=DIRECTION('ref_axis',(1.,0.,0.));
#4344=DIRECTION('',(0.86602540378444,-0.499999999999998,0.));
#4345=DIRECTION('',(0.,-1.,0.));
#4346=DIRECTION('',(-0.86602540378444,-0.499999999999998,0.));
#4347=DIRECTION('center_axis',(-0.866025403784434,0.,-0.500000000000008));
#4348=DIRECTION('ref_axis',(-0.500000000000008,0.,0.866025403784434));
#4349=DIRECTION('',(0.433012701892227,0.499999999999977,-0.750000000000011));
#4350=DIRECTION('',(-0.433012701892221,0.500000000000001,0.749999999999999));
#4351=DIRECTION('center_axis',(0.,-1.,0.));
#4352=DIRECTION('ref_axis',(1.,0.,4.82166445138931E-17));
#4353=DIRECTION('axis',(0.,0.,1.));
#4354=DIRECTION('refdir',(1.,0.,0.));
#4355=DIRECTION('center_axis',(0.,-1.,0.));
#4356=DIRECTION('ref_axis',(0.,0.,-1.));
#4357=DIRECTION('center_axis',(0.,-1.,0.));
#4358=DIRECTION('ref_axis',(0.,0.,-1.));
#4359=DIRECTION('',(0.,-1.,0.));
#4360=DIRECTION('center_axis',(0.,-1.,0.));
#4361=DIRECTION('ref_axis',(0.,0.,-1.));
#4362=DIRECTION('center_axis',(0.,-1.,0.));
#4363=DIRECTION('ref_axis',(0.,0.,-1.));
#4364=DIRECTION('center_axis',(0.,-1.,0.));
#4365=DIRECTION('ref_axis',(0.,0.,-1.));
#4366=DIRECTION('center_axis',(0.,-1.,0.));
#4367=DIRECTION('ref_axis',(0.,0.,-1.));
#4368=DIRECTION('',(8.65956056235495E-17,0.707106781186546,-0.707106781186549));
#4369=DIRECTION('center_axis',(0.,1.,0.));
#4370=DIRECTION('ref_axis',(0.,0.,-1.));
#4371=DIRECTION('center_axis',(0.,1.,0.));
#4372=DIRECTION('ref_axis',(0.,0.,1.));
#4373=DIRECTION('',(0.,-1.,0.));
#4374=DIRECTION('center_axis',(0.,-1.,0.));
#4375=DIRECTION('ref_axis',(0.,0.,-1.));
#4376=DIRECTION('center_axis',(0.,1.,0.));
#4377=DIRECTION('ref_axis',(0.,0.,1.));
#4378=DIRECTION('center_axis',(0.,-1.,0.));
#4379=DIRECTION('ref_axis',(0.,0.,-1.));
#4380=DIRECTION('',(0.,1.,0.));
#4381=DIRECTION('center_axis',(0.,-1.,0.));
#4382=DIRECTION('ref_axis',(0.,0.,-1.));
#4383=DIRECTION('center_axis',(0.,-1.,0.));
#4384=DIRECTION('ref_axis',(0.,0.,-1.));
#4385=DIRECTION('center_axis',(0.,-1.,0.));
#4386=DIRECTION('ref_axis',(0.,0.,-1.));
#4387=DIRECTION('center_axis',(0.,-1.,0.));
#4388=DIRECTION('ref_axis',(0.,0.,-1.));
#4389=DIRECTION('axis',(0.,0.,1.));
#4390=DIRECTION('refdir',(1.,0.,0.));
#4391=DIRECTION('center_axis',(0.,0.,1.));
#4392=DIRECTION('ref_axis',(1.,0.,0.));
#4393=DIRECTION('center_axis',(0.,0.,-1.));
#4394=DIRECTION('ref_axis',(-1.,0.,0.));
#4395=DIRECTION('',(0.,0.,1.));
#4396=DIRECTION('center_axis',(0.,0.,-1.));
#4397=DIRECTION('ref_axis',(-1.,0.,0.));
#4398=DIRECTION('center_axis',(0.,-1.,0.));
#4399=DIRECTION('ref_axis',(0.,0.,-1.));
#4400=DIRECTION('center_axis',(0.,1.,0.));
#4401=DIRECTION('ref_axis',(0.,0.,1.));
#4402=DIRECTION('',(0.,-1.,0.));
#4403=DIRECTION('center_axis',(0.,1.,0.));
#4404=DIRECTION('ref_axis',(0.,0.,1.));
#4405=DIRECTION('center_axis',(0.,1.,0.));
#4406=DIRECTION('ref_axis',(0.,0.,1.));
#4407=DIRECTION('center_axis',(0.,-1.,0.));
#4408=DIRECTION('ref_axis',(-1.,0.,1.83697019872103E-16));
#4409=DIRECTION('center_axis',(0.,1.,0.));
#4410=DIRECTION('ref_axis',(1.,0.,0.));
#4411=DIRECTION('',(0.,-1.,0.));
#4412=DIRECTION('center_axis',(0.,1.,0.));
#4413=DIRECTION('ref_axis',(1.,0.,0.));
#4414=DIRECTION('',(0.,-1.,0.));
#4415=DIRECTION('center_axis',(0.,1.,0.));
#4416=DIRECTION('ref_axis',(0.,0.,1.));
#4417=DIRECTION('',(-1.,0.,0.));
#4418=DIRECTION('',(0.,0.,1.));
#4419=DIRECTION('',(0.,0.,1.));
#4420=DIRECTION('',(-1.,0.,0.));
#4421=DIRECTION('center_axis',(0.,1.,0.));
#4422=DIRECTION('ref_axis',(0.,0.,1.));
#4423=DIRECTION('',(1.,0.,0.));
#4424=DIRECTION('',(0.,0.,1.));
#4425=DIRECTION('',(1.,0.,0.));
#4426=DIRECTION('center_axis',(0.,0.,-1.));
#4427=DIRECTION('ref_axis',(-1.,0.,0.));
#4428=DIRECTION('center_axis',(0.,0.,1.));
#4429=DIRECTION('ref_axis',(-1.,0.,0.));
#4430=DIRECTION('',(1.,0.,0.));
#4431=DIRECTION('center_axis',(0.,0.,1.));
#4432=DIRECTION('ref_axis',(-1.,0.,0.));
#4433=DIRECTION('center_axis',(0.,0.,-1.));
#4434=DIRECTION('ref_axis',(-1.,0.,0.));
#4435=DIRECTION('center_axis',(0.,0.,-1.));
#4436=DIRECTION('ref_axis',(-1.,0.,0.));
#4437=DIRECTION('center_axis',(0.,0.,-1.));
#4438=DIRECTION('ref_axis',(-1.,0.,0.));
#4439=DIRECTION('',(1.,0.,0.));
#4440=DIRECTION('center_axis',(0.,-1.,0.));
#4441=DIRECTION('ref_axis',(-1.,0.,0.));
#4442=DIRECTION('',(0.,0.,-1.));
#4443=DIRECTION('',(0.,0.,1.));
#4444=DIRECTION('center_axis',(0.,0.,-1.));
#4445=DIRECTION('ref_axis',(-1.,0.,0.));
#4446=DIRECTION('center_axis',(0.,0.,-1.));
#4447=DIRECTION('ref_axis',(1.,1.22464679914735E-16,0.));
#4448=DIRECTION('axis',(0.,0.,1.));
#4449=DIRECTION('refdir',(1.,0.,0.));
#4450=DIRECTION('center_axis',(0.,0.,1.));
#4451=DIRECTION('ref_axis',(1.,0.,0.));
#4452=DIRECTION('center_axis',(0.,0.,-1.));
#4453=DIRECTION('ref_axis',(-1.,0.,0.));
#4454=DIRECTION('',(0.,0.,1.));
#4455=DIRECTION('center_axis',(0.,0.,1.));
#4456=DIRECTION('ref_axis',(1.,0.,0.));
#4457=DIRECTION('center_axis',(0.,0.,1.));
#4458=DIRECTION('ref_axis',(1.,0.,0.));
#4459=DIRECTION('center_axis',(0.,0.,1.));
#4460=DIRECTION('ref_axis',(1.,0.,0.));
#4461=DIRECTION('',(0.,0.,1.));
#4462=DIRECTION('center_axis',(0.,0.,1.));
#4463=DIRECTION('ref_axis',(1.,0.,0.));
#4464=DIRECTION('center_axis',(0.,0.,1.));
#4465=DIRECTION('ref_axis',(1.,0.,0.));
#4466=DIRECTION('center_axis',(0.,0.,-1.));
#4467=DIRECTION('ref_axis',(-1.,0.,0.));
#4468=DIRECTION('',(0.,0.,1.));
#4469=DIRECTION('center_axis',(0.,0.,1.));
#4470=DIRECTION('ref_axis',(1.,0.,0.));
#4471=DIRECTION('center_axis',(0.,0.,1.));
#4472=DIRECTION('ref_axis',(1.,0.,0.));
#4473=DIRECTION('center_axis',(0.,0.,1.));
#4474=DIRECTION('ref_axis',(1.,0.,0.));
#4475=DIRECTION('',(0.,0.,1.));
#4476=DIRECTION('center_axis',(0.,0.,1.));
#4477=DIRECTION('ref_axis',(1.,0.,0.));
#4478=DIRECTION('center_axis',(0.,0.,-1.));
#4479=DIRECTION('ref_axis',(-1.,0.,0.));
#4480=DIRECTION('center_axis',(0.,0.,1.));
#4481=DIRECTION('ref_axis',(-1.,0.,0.));
#4482=DIRECTION('',(0.,0.,1.));
#4483=DIRECTION('center_axis',(0.,0.,-1.));
#4484=DIRECTION('ref_axis',(-1.,0.,0.));
#4485=DIRECTION('',(0.,0.,-1.));
#4486=DIRECTION('center_axis',(0.415719046892318,0.909493086312888,0.));
#4487=DIRECTION('ref_axis',(-0.909493086312888,0.415719046892318,0.));
#4488=DIRECTION('',(0.909493086312888,-0.415719046892318,0.));
#4489=DIRECTION('',(0.,0.,1.));
#4490=DIRECTION('',(0.909493086312888,-0.415719046892318,0.));
#4491=DIRECTION('',(0.,0.,1.));
#4492=DIRECTION('',(0.909493086312888,-0.415719046892318,0.));
#4493=DIRECTION('',(0.,0.,-1.));
#4494=DIRECTION('',(0.909493086312888,-0.415719046892318,0.));
#4495=DIRECTION('',(0.,0.,-1.));
#4496=DIRECTION('center_axis',(0.909493086312887,-0.41571904689232,0.));
#4497=DIRECTION('ref_axis',(0.41571904689232,0.909493086312887,0.));
#4498=DIRECTION('',(-0.41571904689232,-0.909493086312887,0.));
#4499=DIRECTION('',(0.,0.,-1.));
#4500=DIRECTION('',(-0.41571904689232,-0.909493086312887,0.));
#4501=DIRECTION('center_axis',(0.415719046892318,0.909493086312888,0.));
#4502=DIRECTION('ref_axis',(-0.909493086312888,0.415719046892318,0.));
#4503=DIRECTION('',(0.909493086312888,-0.415719046892318,0.));
#4504=DIRECTION('',(0.909493086312888,-0.415719046892318,0.));
#4505=DIRECTION('',(0.,0.,1.));
#4506=DIRECTION('',(0.909493086312888,-0.415719046892318,0.));
#4507=DIRECTION('',(0.,0.,1.));
#4508=DIRECTION('',(0.909493086312888,-0.415719046892318,0.));
#4509=DIRECTION('',(0.,0.,-1.));
#4510=DIRECTION('center_axis',(-0.42949307237204,0.903070152748072,0.));
#4511=DIRECTION('ref_axis',(-0.903070152748072,-0.42949307237204,0.));
#4512=DIRECTION('',(0.903070152748072,0.42949307237204,0.));
#4513=DIRECTION('',(0.903070152748072,0.42949307237204,0.));
#4514=DIRECTION('center_axis',(-0.42949307237204,0.903070152748072,0.));
#4515=DIRECTION('ref_axis',(-0.903070152748072,-0.42949307237204,0.));
#4516=DIRECTION('',(0.903070152748072,0.42949307237204,0.));
#4517=DIRECTION('',(0.903070152748072,0.42949307237204,0.));
#4518=DIRECTION('center_axis',(0.,0.,-1.));
#4519=DIRECTION('ref_axis',(-1.,0.,0.));
#4520=DIRECTION('center_axis',(0.,0.,-1.));
#4521=DIRECTION('ref_axis',(-1.,0.,0.));
#4522=DIRECTION('',(0.415719046892314,0.90949308631289,0.));
#4523=DIRECTION('center_axis',(-0.90949308631289,0.415719046892314,0.));
#4524=DIRECTION('ref_axis',(-0.415719046892314,-0.90949308631289,0.));
#4525=DIRECTION('',(0.415719046892314,0.90949308631289,0.));
#4526=DIRECTION('center_axis',(-0.42949307237204,0.903070152748072,0.));
#4527=DIRECTION('ref_axis',(-0.903070152748072,-0.42949307237204,0.));
#4528=DIRECTION('',(0.903070152748072,0.42949307237204,0.));
#4529=DIRECTION('',(0.903070152748072,0.42949307237204,0.));
#4530=DIRECTION('',(0.,0.,-1.));
#4531=DIRECTION('center_axis',(-0.42949307237204,0.903070152748072,0.));
#4532=DIRECTION('ref_axis',(-0.903070152748072,-0.42949307237204,0.));
#4533=DIRECTION('',(0.903070152748072,0.42949307237204,0.));
#4534=DIRECTION('',(0.903070152748072,0.42949307237204,0.));
#4535=DIRECTION('',(0.,0.,1.));
#4536=DIRECTION('center_axis',(0.,0.,1.));
#4537=DIRECTION('ref_axis',(-1.,0.,0.));
#4538=DIRECTION('center_axis',(0.,0.,1.));
#4539=DIRECTION('ref_axis',(-1.,0.,0.));
#4540=DIRECTION('center_axis',(0.,0.,1.));
#4541=DIRECTION('ref_axis',(-1.,0.,0.));
#4542=DIRECTION('center_axis',(0.,0.,-1.));
#4543=DIRECTION('ref_axis',(-1.,0.,0.));
#4544=DIRECTION('center_axis',(0.,0.,-1.));
#4545=DIRECTION('ref_axis',(-0.903070152748072,-0.429493072372039,0.));
#4546=DIRECTION('axis',(0.,0.,1.));
#4547=DIRECTION('refdir',(1.,0.,0.));
#4548=DIRECTION('center_axis',(9.93970987904536E-15,-0.0655103873942315,
0.99785188737781));
#4549=DIRECTION('ref_axis',(-2.5496135091776E-31,0.99785188737781,0.0655103873942315));
#4550=DIRECTION('center_axis',(-9.93970987904536E-15,0.0655103873942315,
-0.99785188737781));
#4551=DIRECTION('ref_axis',(-2.5496135091776E-31,0.99785188737781,0.0655103873942315));
#4552=DIRECTION('center_axis',(9.93970987904537E-15,-0.0655103873942315,
0.99785188737781));
#4553=DIRECTION('ref_axis',(-1.56056201915558E-32,-0.99785188737781,-0.0655103873942315));
#4554=DIRECTION('center_axis',(-9.93970987904536E-15,0.0655103873942315,
-0.99785188737781));
#4555=DIRECTION('ref_axis',(-2.5496135091776E-31,0.99785188737781,0.0655103873942315));
#4556=DIRECTION('',(1.,0.,-9.96110745971056E-15));
#4557=DIRECTION('center_axis',(9.93970987904536E-15,-0.0655103873942315,
0.99785188737781));
#4558=DIRECTION('ref_axis',(-2.5496135091776E-31,0.99785188737781,0.0655103873942315));
#4559=DIRECTION('center_axis',(9.93970987904537E-15,-0.0655103873942315,
0.99785188737781));
#4560=DIRECTION('ref_axis',(-1.56056201915558E-32,-0.99785188737781,-0.0655103873942315));
#4561=DIRECTION('center_axis',(0.,-1.,0.));
#4562=DIRECTION('ref_axis',(-1.,0.,0.));
#4563=DIRECTION('axis',(0.,0.,1.));
#4564=DIRECTION('refdir',(1.,0.,0.));
#4565=DIRECTION('center_axis',(0.,0.,1.));
#4566=DIRECTION('ref_axis',(1.,0.,0.));
#4567=DIRECTION('center_axis',(0.,0.,-1.));
#4568=DIRECTION('ref_axis',(1.,0.,0.));
#4569=DIRECTION('',(0.,0.,1.));
#4570=DIRECTION('center_axis',(0.,0.,1.));
#4571=DIRECTION('ref_axis',(1.,0.,0.));
#4572=DIRECTION('center_axis',(0.,0.,1.));
#4573=DIRECTION('ref_axis',(1.,0.,0.));
#4574=DIRECTION('center_axis',(0.,0.,-1.));
#4575=DIRECTION('ref_axis',(-1.,0.,0.));
#4576=DIRECTION('center_axis',(0.,0.,1.));
#4577=DIRECTION('ref_axis',(-1.,0.,0.));
#4578=DIRECTION('',(0.81915204428899,-1.00317192905352E-16,-0.573576436351048));
#4579=DIRECTION('center_axis',(0.,0.,1.));
#4580=DIRECTION('ref_axis',(-1.,0.,0.));
#4581=DIRECTION('center_axis',(0.,0.,1.));
#4582=DIRECTION('ref_axis',(1.,0.,0.));
#4583=DIRECTION('center_axis',(0.,0.,-1.));
#4584=DIRECTION('ref_axis',(1.,0.,0.));
#4585=DIRECTION('',(-0.819152044288991,-1.00317192905352E-16,0.573576436351046));
#4586=DIRECTION('center_axis',(0.,0.,1.));
#4587=DIRECTION('ref_axis',(1.,0.,0.));
#4588=DIRECTION('center_axis',(0.,0.,-1.));
#4589=DIRECTION('ref_axis',(-1.,0.,0.));
#4590=DIRECTION('center_axis',(0.,0.,1.));
#4591=DIRECTION('ref_axis',(1.,0.,0.));
#4592=DIRECTION('',(-0.939692620785915,1.15079156022786E-16,0.342020143325652));
#4593=DIRECTION('center_axis',(0.,0.,1.));
#4594=DIRECTION('ref_axis',(1.,0.,0.));
#4595=DIRECTION('center_axis',(0.,0.,1.));
#4596=DIRECTION('ref_axis',(1.,0.,0.));
#4597=DIRECTION('center_axis',(1.22464679914735E-16,-1.,0.));
#4598=DIRECTION('ref_axis',(-1.,-1.22464679914735E-16,0.));
#4599=DIRECTION('center_axis',(0.,0.,1.));
#4600=DIRECTION('ref_axis',(1.,0.,0.));
#4601=DIRECTION('center_axis',(0.,0.,1.));
#4602=DIRECTION('ref_axis',(1.,0.,0.));
#4603=DIRECTION('',(0.,0.,1.));
#4604=DIRECTION('center_axis',(-0.5,0.866025403784438,0.));
#4605=DIRECTION('ref_axis',(-0.866025403784438,-0.5,0.));
#4606=DIRECTION('',(0.,0.,1.));
#4607=DIRECTION('',(0.,0.,1.));
#4608=DIRECTION('center_axis',(0.5,0.866025403784438,0.));
#4609=DIRECTION('ref_axis',(-0.866025403784438,0.5,0.));
#4610=DIRECTION('',(0.,0.,1.));
#4611=DIRECTION('center_axis',(-1.,0.,0.));
#4612=DIRECTION('ref_axis',(0.,0.,1.));
#4613=DIRECTION('',(0.,0.,1.));
#4614=DIRECTION('center_axis',(0.5,-0.866025403784438,0.));
#4615=DIRECTION('ref_axis',(0.866025403784438,0.5,0.));
#4616=DIRECTION('',(0.,0.,1.));
#4617=DIRECTION('center_axis',(-0.5,-0.866025403784438,0.));
#4618=DIRECTION('ref_axis',(0.866025403784438,-0.5,0.));
#4619=DIRECTION('',(0.,0.,1.));
#4620=DIRECTION('center_axis',(-1.,0.,0.));
#4621=DIRECTION('ref_axis',(0.,0.,1.));
#4622=DIRECTION('center_axis',(0.,0.,1.));
#4623=DIRECTION('ref_axis',(1.,0.,0.));
#4624=DIRECTION('center_axis',(0.,0.,1.));
#4625=DIRECTION('ref_axis',(1.,0.,0.));
#4626=DIRECTION('center_axis',(0.,0.,1.));
#4627=DIRECTION('ref_axis',(1.,0.,0.));
#4628=DIRECTION('center_axis',(0.,0.,1.));
#4629=DIRECTION('ref_axis',(1.,0.,0.));
#4630=DIRECTION('center_axis',(0.,0.,1.));
#4631=DIRECTION('ref_axis',(1.,0.,0.));
#4632=DIRECTION('center_axis',(0.,0.,1.));
#4633=DIRECTION('ref_axis',(1.,0.,0.));
#4634=DIRECTION('center_axis',(0.,0.,1.));
#4635=DIRECTION('ref_axis',(1.,0.,0.));
#4636=DIRECTION('center_axis',(0.,0.,1.));
#4637=DIRECTION('ref_axis',(1.,0.,0.));
#4638=DIRECTION('center_axis',(0.,0.,-1.));
#4639=DIRECTION('ref_axis',(-1.,0.,0.));
#4640=DIRECTION('center_axis',(0.,0.,-1.));
#4641=DIRECTION('ref_axis',(-1.,0.,0.));
#4642=DIRECTION('center_axis',(0.,0.,-1.));
#4643=DIRECTION('ref_axis',(-1.,0.,0.));
#4644=DIRECTION('center_axis',(0.,0.,-1.));
#4645=DIRECTION('ref_axis',(-1.,0.,0.));
#4646=DIRECTION('center_axis',(0.,0.,-1.));
#4647=DIRECTION('ref_axis',(-1.,0.,0.));
#4648=DIRECTION('center_axis',(0.,0.,-1.));
#4649=DIRECTION('ref_axis',(-1.,0.,0.));
#4650=DIRECTION('axis',(0.,0.,1.));
#4651=DIRECTION('refdir',(1.,0.,0.));
#4652=DIRECTION('center_axis',(0.,0.,1.));
#4653=DIRECTION('ref_axis',(1.,0.,0.));
#4654=DIRECTION('center_axis',(0.,0.,-1.));
#4655=DIRECTION('ref_axis',(-1.,0.,0.));
#4656=DIRECTION('',(0.,0.,-1.));
#4657=DIRECTION('center_axis',(0.,0.,-1.));
#4658=DIRECTION('ref_axis',(-1.,0.,0.));
#4659=DIRECTION('center_axis',(0.,0.,-1.));
#4660=DIRECTION('ref_axis',(-1.,0.,0.));
#4661=DIRECTION('center_axis',(0.,0.,1.));
#4662=DIRECTION('ref_axis',(1.,0.,0.));
#4663=DIRECTION('',(0.,0.,1.));
#4664=DIRECTION('center_axis',(0.,0.,1.));
#4665=DIRECTION('ref_axis',(1.,0.,0.));
#4666=DIRECTION('center_axis',(0.,0.,1.));
#4667=DIRECTION('ref_axis',(1.,0.,0.));
#4668=DIRECTION('center_axis',(0.,0.,1.));
#4669=DIRECTION('ref_axis',(1.,0.,0.));
#4670=DIRECTION('',(0.,0.,-1.));
#4671=DIRECTION('center_axis',(0.,0.,-1.));
#4672=DIRECTION('ref_axis',(1.,0.,0.));
#4673=DIRECTION('center_axis',(0.,0.,1.));
#4674=DIRECTION('ref_axis',(1.,0.,0.));
#4675=DIRECTION('center_axis',(0.,0.,1.));
#4676=DIRECTION('ref_axis',(1.,0.,0.));
#4677=DIRECTION('center_axis',(0.,0.,-1.));
#4678=DIRECTION('ref_axis',(-1.,0.,0.));
#4679=DIRECTION('center_axis',(0.,0.,-1.));
#4680=DIRECTION('ref_axis',(-1.,0.,0.));
#4681=DIRECTION('',(0.,0.,1.));
#4682=DIRECTION('',(1.,0.,0.));
#4683=DIRECTION('',(0.,0.,1.));
#4684=DIRECTION('',(1.,0.,0.));
#4685=DIRECTION('',(0.,0.,1.));
#4686=DIRECTION('',(1.,0.,0.));
#4687=DIRECTION('',(0.,0.,1.));
#4688=DIRECTION('',(1.,0.,0.));
#4689=DIRECTION('',(0.,0.,1.));
#4690=DIRECTION('',(1.,0.,0.));
#4691=DIRECTION('',(0.,0.,1.));
#4692=DIRECTION('',(1.,0.,0.));
#4693=DIRECTION('',(0.,0.,1.));
#4694=DIRECTION('',(1.,0.,0.));
#4695=DIRECTION('',(0.,0.,1.));
#4696=DIRECTION('',(1.,0.,0.));
#4697=DIRECTION('',(0.,-1.,0.));
#4698=DIRECTION('',(1.,0.,0.));
#4699=DIRECTION('',(0.,0.,1.));
#4700=DIRECTION('',(1.,0.,0.));
#4701=CARTESIAN_POINT('',(0.,0.,0.));
#4702=CARTESIAN_POINT('',(0.,0.,0.));
#4703=CARTESIAN_POINT('Origin',(0.,10.,0.));
#4704=CARTESIAN_POINT('',(-3.67394039744206E-15,10.,30.));
#4705=CARTESIAN_POINT('Origin',(0.,10.,0.));
#4706=CARTESIAN_POINT('',(-3.67394039744206E-15,1.11022302462516E-15,30.));
#4707=CARTESIAN_POINT('',(-3.67394039744206E-15,10.,30.));
#4708=CARTESIAN_POINT('Origin',(0.,0.,0.));
#4709=CARTESIAN_POINT('Origin',(0.,10.,0.));
#4710=CARTESIAN_POINT('',(39.5474398665704,10.,-6.));
#4711=CARTESIAN_POINT('',(-39.5474398665704,10.,-5.99999999999999));
#4712=CARTESIAN_POINT('Origin',(0.,10.,0.));
#4713=CARTESIAN_POINT('',(39.5474398665704,0.,-6.));
#4714=CARTESIAN_POINT('',(39.5474398665704,10.,-6.));
#4715=CARTESIAN_POINT('',(-39.5474398665704,0.,-5.99999999999999));
#4716=CARTESIAN_POINT('Origin',(0.,0.,0.));
#4717=CARTESIAN_POINT('',(-39.5474398665704,10.,-5.99999999999999));
#4718=CARTESIAN_POINT('Origin',(0.,10.,0.));
#4719=CARTESIAN_POINT('',(-37.,10.,-5.99999999999999));
#4720=CARTESIAN_POINT('',(0.,10.,-5.99999999999999));
#4721=CARTESIAN_POINT('',(-37.,10.,6.00000000000001));
#4722=CARTESIAN_POINT('',(-37.,10.,0.));
#4723=CARTESIAN_POINT('',(-39.5474398665704,10.,6.00000000000001));
#4724=CARTESIAN_POINT('',(0.,10.,6.00000000000001));
#4725=CARTESIAN_POINT('',(39.5474398665704,10.,6.));
#4726=CARTESIAN_POINT('Origin',(0.,10.,0.));
#4727=CARTESIAN_POINT('',(37.,10.,6.00000000000001));
#4728=CARTESIAN_POINT('',(1.73472347597681E-15,10.,6.00000000000002));
#4729=CARTESIAN_POINT('',(37.,10.,-6.));
#4730=CARTESIAN_POINT('',(37.,10.,0.));
#4731=CARTESIAN_POINT('',(-1.7347234759768E-15,10.,-5.99999999999999));
#4732=CARTESIAN_POINT('Origin',(0.,10.,0.));
#4733=CARTESIAN_POINT('',(-39.5474398665704,0.,6.00000000000001));
#4734=CARTESIAN_POINT('',(-39.5474398665704,10.,6.00000000000001));
#4735=CARTESIAN_POINT('',(39.5474398665704,0.,6.));
#4736=CARTESIAN_POINT('Origin',(0.,0.,0.));
#4737=CARTESIAN_POINT('',(39.5474398665704,10.,6.));
#4738=CARTESIAN_POINT('Origin',(0.,0.,0.));
#4739=CARTESIAN_POINT('',(-43.,0.,6.00000000000001));
#4740=CARTESIAN_POINT('',(-43.,0.,6.00000000000001));
#4741=CARTESIAN_POINT('',(-43.,0.,-5.99999999999999));
#4742=CARTESIAN_POINT('',(-43.,0.,6.00000000000001));
#4743=CARTESIAN_POINT('',(-43.,0.,-5.99999999999999));
#4744=CARTESIAN_POINT('',(43.,0.,-6.));
#4745=CARTESIAN_POINT('',(43.,0.,-6.));
#4746=CARTESIAN_POINT('',(43.,0.,6.));
#4747=CARTESIAN_POINT('',(43.,0.,6.));
#4748=CARTESIAN_POINT('',(43.,0.,6.));
#4749=CARTESIAN_POINT('Origin',(43.,300.,6.));
#4750=CARTESIAN_POINT('',(43.,300.,-6.));
#4751=CARTESIAN_POINT('',(43.,300.,-6.));
#4752=CARTESIAN_POINT('',(43.,300.,6.));
#4753=CARTESIAN_POINT('',(43.,300.,6.));
#4754=CARTESIAN_POINT('',(43.,300.,6.));
#4755=CARTESIAN_POINT('Origin',(43.,300.,-6.));
#4756=CARTESIAN_POINT('',(37.,300.,-6.));
#4757=CARTESIAN_POINT('',(37.,300.,-6.));
#4758=CARTESIAN_POINT('',(43.,300.,-6.));
#4759=CARTESIAN_POINT('Origin',(37.,300.,6.00000000000001));
#4760=CARTESIAN_POINT('',(37.,300.,6.00000000000001));
#4761=CARTESIAN_POINT('',(37.,300.,6.00000000000001));
#4762=CARTESIAN_POINT('',(37.,300.,6.00000000000001));
#4763=CARTESIAN_POINT('Origin',(43.,300.,6.));
#4764=CARTESIAN_POINT('',(43.,300.,6.));
#4765=CARTESIAN_POINT('Origin',(0.,300.,0.));
#4766=CARTESIAN_POINT('Origin',(-37.,300.,6.00000000000001));
#4767=CARTESIAN_POINT('',(-37.,300.,-5.99999999999999));
#4768=CARTESIAN_POINT('',(-37.,300.,-5.99999999999999));
#4769=CARTESIAN_POINT('',(-37.,300.,6.00000000000001));
#4770=CARTESIAN_POINT('',(-37.,300.,6.00000000000001));
#4771=CARTESIAN_POINT('',(-37.,300.,6.00000000000001));
#4772=CARTESIAN_POINT('Origin',(-43.,300.,-5.99999999999999));
#4773=CARTESIAN_POINT('',(-43.,300.,-5.99999999999999));
#4774=CARTESIAN_POINT('',(-43.,300.,-5.99999999999999));
#4775=CARTESIAN_POINT('',(-43.,300.,-5.99999999999999));
#4776=CARTESIAN_POINT('Origin',(-43.,300.,6.00000000000001));
#4777=CARTESIAN_POINT('',(-43.,300.,6.00000000000001));
#4778=CARTESIAN_POINT('',(-43.,300.,6.00000000000001));
#4779=CARTESIAN_POINT('',(-43.,300.,6.00000000000001));
#4780=CARTESIAN_POINT('Origin',(-43.,300.,6.00000000000001));
#4781=CARTESIAN_POINT('',(-43.,300.,6.00000000000001));
#4782=CARTESIAN_POINT('Origin',(0.,300.,0.));
#4783=CARTESIAN_POINT('',(0.,0.,0.));
#4784=CARTESIAN_POINT('Origin',(32.,329.539392014169,6.2));
#4785=CARTESIAN_POINT('',(30.,329.539392014169,-4.));
#4786=CARTESIAN_POINT('Origin',(32.,329.539392014169,-4.));
#4787=CARTESIAN_POINT('',(30.,329.539392014169,4.));
#4788=CARTESIAN_POINT('',(30.,329.539392014169,6.2));
#4789=CARTESIAN_POINT('Origin',(32.,329.539392014169,4.));
#4790=CARTESIAN_POINT('Origin',(0.,275.,0.));
#4791=CARTESIAN_POINT('',(-7.34788079488412E-16,275.,-6.));
#4792=CARTESIAN_POINT('Origin',(0.,275.,0.));
#4793=CARTESIAN_POINT('',(-7.34788079488412E-16,285.,-6.));
#4794=CARTESIAN_POINT('',(-7.34788079488412E-16,275.,-6.));
#4795=CARTESIAN_POINT('Origin',(0.,285.,0.));
#4796=CARTESIAN_POINT('Origin',(0.,275.,0.));
#4797=CARTESIAN_POINT('',(-7.34788079488412E-16,335.,-6.));
#4798=CARTESIAN_POINT('Origin',(0.,335.,0.));
#4799=CARTESIAN_POINT('',(-7.34788079488412E-16,345.,-6.));
#4800=CARTESIAN_POINT('',(-7.34788079488412E-16,275.,-6.));
#4801=CARTESIAN_POINT('Origin',(0.,345.,0.));
#4802=CARTESIAN_POINT('Origin',(0.,335.,0.));
#4803=CARTESIAN_POINT('',(-11.842719282327,335.,4.));
#4804=CARTESIAN_POINT('',(11.842719282327,335.,4.));
#4805=CARTESIAN_POINT('Origin',(0.,335.,0.));
#4806=CARTESIAN_POINT('',(11.842719282327,345.,4.));
#4807=CARTESIAN_POINT('',(11.842719282327,335.,4.));
#4808=CARTESIAN_POINT('',(-11.842719282327,345.,4.));
#4809=CARTESIAN_POINT('Origin',(0.,345.,0.));
#4810=CARTESIAN_POINT('',(-11.842719282327,335.,4.));
#4811=CARTESIAN_POINT('Origin',(0.,275.,0.));
#4812=CARTESIAN_POINT('',(-11.842719282327,275.,4.));
#4813=CARTESIAN_POINT('',(11.842719282327,275.,4.));
#4814=CARTESIAN_POINT('Origin',(0.,275.,0.));
#4815=CARTESIAN_POINT('',(11.842719282327,285.,4.));
#4816=CARTESIAN_POINT('',(11.842719282327,275.,4.));
#4817=CARTESIAN_POINT('',(-11.842719282327,285.,4.));
#4818=CARTESIAN_POINT('Origin',(0.,285.,0.));
#4819=CARTESIAN_POINT('',(-11.842719282327,275.,4.));
#4820=CARTESIAN_POINT('Origin',(29.,345.,-5.99999999999999));
#4821=CARTESIAN_POINT('',(29.,300.,4.));
#4822=CARTESIAN_POINT('',(29.,320.,4.));
#4823=CARTESIAN_POINT('',(29.,345.,4.));
#4824=CARTESIAN_POINT('',(29.,320.,-4.));
#4825=CARTESIAN_POINT('',(29.,320.,-5.99999999999999));
#4826=CARTESIAN_POINT('',(29.,300.,-4.));
#4827=CARTESIAN_POINT('',(29.,345.,-4.));
#4828=CARTESIAN_POINT('',(29.,300.,-6.));
#4829=CARTESIAN_POINT('',(29.,300.,-4.));
#4830=CARTESIAN_POINT('',(29.,275.,-5.99999999999999));
#4831=CARTESIAN_POINT('',(29.,345.,-5.99999999999999));
#4832=CARTESIAN_POINT('',(29.,275.,-4.));
#4833=CARTESIAN_POINT('',(29.,275.,-5.99999999999999));
#4834=CARTESIAN_POINT('',(29.,285.,-4.));
#4835=CARTESIAN_POINT('',(29.,285.,-4.));
#4836=CARTESIAN_POINT('',(29.,285.,4.));
#4837=CARTESIAN_POINT('',(29.,285.,0.));
#4838=CARTESIAN_POINT('',(29.,275.,4.));
#4839=CARTESIAN_POINT('',(29.,285.,4.));
#4840=CARTESIAN_POINT('',(29.,275.,6.00000000000001));
#4841=CARTESIAN_POINT('',(29.,275.,-5.99999999999999));
#4842=CARTESIAN_POINT('',(29.,300.,6.));
#4843=CARTESIAN_POINT('',(29.,345.,6.00000000000001));
#4844=CARTESIAN_POINT('',(29.,300.,4.));
#4845=CARTESIAN_POINT('Origin',(37.,345.,6.));
#4846=CARTESIAN_POINT('',(37.,300.,6.));
#4847=CARTESIAN_POINT('',(-37.001,300.,6.));
#4848=CARTESIAN_POINT('',(37.,275.,6.));
#4849=CARTESIAN_POINT('',(37.,275.,6.));
#4850=CARTESIAN_POINT('',(37.,345.,6.));
#4851=CARTESIAN_POINT('Origin',(0.,345.,0.));
#4852=CARTESIAN_POINT('',(63.,345.,4.));
#4853=CARTESIAN_POINT('',(-37.,345.,4.));
#4854=CARTESIAN_POINT('',(63.,345.,-4.));
#4855=CARTESIAN_POINT('',(63.,345.,4.));
#4856=CARTESIAN_POINT('',(11.842719282327,345.,-4.));
#4857=CARTESIAN_POINT('',(-37.,345.,-4.));
#4858=CARTESIAN_POINT('',(-11.842719282327,345.,-4.));
#4859=CARTESIAN_POINT('Origin',(0.,345.,0.));
#4860=CARTESIAN_POINT('',(-29.,345.,-4.));
#4861=CARTESIAN_POINT('',(-37.,345.,-4.));
#4862=CARTESIAN_POINT('',(-29.,345.,-5.99999999999999));
#4863=CARTESIAN_POINT('',(-29.,345.,-5.99999999999999));
#4864=CARTESIAN_POINT('',(-37.,345.,-5.99999999999999));
#4865=CARTESIAN_POINT('',(-37.,345.,-5.99999999999999));
#4866=CARTESIAN_POINT('',(-37.,345.,6.00000000000001));
#4867=CARTESIAN_POINT('',(-37.,345.,-5.99999999999999));
#4868=CARTESIAN_POINT('',(-29.,345.,6.00000000000001));
#4869=CARTESIAN_POINT('',(-37.,345.,6.00000000000001));
#4870=CARTESIAN_POINT('',(-29.,345.,4.));
#4871=CARTESIAN_POINT('',(-29.,345.,-5.99999999999999));
#4872=CARTESIAN_POINT('',(-37.,345.,4.));
#4873=CARTESIAN_POINT('Origin',(0.,0.,4.));
#4874=CARTESIAN_POINT('',(-29.,335.,4.));
#4875=CARTESIAN_POINT('',(-37.,335.,4.));
#4876=CARTESIAN_POINT('',(-29.,345.,4.));
#4877=CARTESIAN_POINT('Origin',(0.,0.,-4.));
#4878=CARTESIAN_POINT('',(-11.842719282327,335.,-4.));
#4879=CARTESIAN_POINT('',(-11.842719282327,335.,-4.));
#4880=CARTESIAN_POINT('',(-29.,335.,-4.));
#4881=CARTESIAN_POINT('',(-37.,335.,-4.));
#4882=CARTESIAN_POINT('',(-29.,345.,-4.));
#4883=CARTESIAN_POINT('Origin',(37.,285.,-4.));
#4884=CARTESIAN_POINT('',(37.,335.,-4.));
#4885=CARTESIAN_POINT('',(37.,335.,4.));
#4886=CARTESIAN_POINT('',(37.,335.,-4.));
#4887=CARTESIAN_POINT('',(37.,300.,4.));
#4888=CARTESIAN_POINT('',(37.,345.,4.));
#4889=CARTESIAN_POINT('',(37.,300.,4.));
#4890=CARTESIAN_POINT('',(37.,275.,-6.));
#4891=CARTESIAN_POINT('',(37.,275.,-4.));
#4892=CARTESIAN_POINT('',(37.,300.,-6.));
#4893=CARTESIAN_POINT('',(37.,345.,-6.));
#4894=CARTESIAN_POINT('',(37.,300.,-4.));
#4895=CARTESIAN_POINT('',(37.,300.,-4.));
#4896=CARTESIAN_POINT('',(37.,345.,-4.));
#4897=CARTESIAN_POINT('Origin',(-29.,345.,-5.99999999999999));
#4898=CARTESIAN_POINT('',(-29.,275.,6.00000000000001));
#4899=CARTESIAN_POINT('',(-29.,345.,6.00000000000001));
#4900=CARTESIAN_POINT('',(-29.,275.,4.));
#4901=CARTESIAN_POINT('',(-29.,275.,-5.99999999999999));
#4902=CARTESIAN_POINT('',(-29.,285.,4.));
#4903=CARTESIAN_POINT('',(-29.,285.,4.));
#4904=CARTESIAN_POINT('',(-29.,285.,-4.));
#4905=CARTESIAN_POINT('',(-29.,285.,0.));
#4906=CARTESIAN_POINT('',(-29.,275.,-4.));
#4907=CARTESIAN_POINT('',(-29.,285.,-4.));
#4908=CARTESIAN_POINT('',(-29.,275.,-5.99999999999999));
#4909=CARTESIAN_POINT('',(-29.,275.,-5.99999999999999));
#4910=CARTESIAN_POINT('',(-29.,345.,-5.99999999999999));
#4911=CARTESIAN_POINT('',(-29.,335.,-5.99999999999999));
#4912=CARTESIAN_POINT('Origin',(-37.,285.,4.));
#4913=CARTESIAN_POINT('',(-37.,275.,4.));
#4914=CARTESIAN_POINT('',(-37.,285.,4.));
#4915=CARTESIAN_POINT('Origin',(-37.,285.,-4.));
#4916=CARTESIAN_POINT('',(-11.842719282327,275.,-4.));
#4917=CARTESIAN_POINT('',(-37.,275.,-4.));
#4918=CARTESIAN_POINT('',(-11.842719282327,285.,-4.));
#4919=CARTESIAN_POINT('',(-37.,285.,-4.));
#4920=CARTESIAN_POINT('',(-11.842719282327,275.,-4.));
#4921=CARTESIAN_POINT('Origin',(-37.,285.,4.));
#4922=CARTESIAN_POINT('',(-37.,285.,4.));
#4923=CARTESIAN_POINT('',(-37.,275.,4.));
#4924=CARTESIAN_POINT('Origin',(-37.,285.,-4.));
#4925=CARTESIAN_POINT('',(11.842719282327,285.,-4.));
#4926=CARTESIAN_POINT('',(-37.,285.,-4.));
#4927=CARTESIAN_POINT('',(11.842719282327,275.,-4.));
#4928=CARTESIAN_POINT('',(-37.,275.,-4.));
#4929=CARTESIAN_POINT('',(11.842719282327,275.,-4.));
#4930=CARTESIAN_POINT('Origin',(0.,285.,0.));
#4931=CARTESIAN_POINT('Origin',(0.,285.,0.));
#4932=CARTESIAN_POINT('Origin',(-37.,285.,4.));
#4933=CARTESIAN_POINT('',(-37.,275.,6.00000000000001));
#4934=CARTESIAN_POINT('',(-37.,345.,6.00000000000001));
#4935=CARTESIAN_POINT('',(-37.,275.,-5.99999999999999));
#4936=CARTESIAN_POINT('',(-37.,345.,-5.99999999999999));
#4937=CARTESIAN_POINT('',(-37.,275.,4.));
#4938=CARTESIAN_POINT('Origin',(0.,275.,0.));
#4939=CARTESIAN_POINT('',(-37.,275.,6.00000000000001));
#4940=CARTESIAN_POINT('',(-37.,275.,-5.99999999999999));
#4941=CARTESIAN_POINT('Origin',(0.,275.,0.));
#4942=CARTESIAN_POINT('',(37.,275.,-6.));
#4943=CARTESIAN_POINT('Origin',(0.,275.,0.));
#4944=CARTESIAN_POINT('Origin',(37.,345.,-6.));
#4945=CARTESIAN_POINT('',(-37.001,300.,-6.));
#4946=CARTESIAN_POINT('Origin',(-37.,345.,6.00000000000001));
#4947=CARTESIAN_POINT('Origin',(-37.,345.,-5.99999999999999));
#4948=CARTESIAN_POINT('Origin',(0.,0.,4.));
#4949=CARTESIAN_POINT('',(22.,335.,4.));
#4950=CARTESIAN_POINT('',(22.,329.539392014169,4.));
#4951=CARTESIAN_POINT('',(22.,335.,4.));
#4952=CARTESIAN_POINT('Origin',(32.,329.539392014169,4.));
#4953=CARTESIAN_POINT('',(-37.001,300.,4.));
#4954=CARTESIAN_POINT('',(63.8748866352591,335.,4.));
#4955=CARTESIAN_POINT('',(-37.,335.,4.));
#4956=CARTESIAN_POINT('',(143.521102017646,349.043776683232,4.));
#4957=CARTESIAN_POINT('',(64.7364817766693,335.151922469878,4.));
#4958=CARTESIAN_POINT('',(141.784620240977,358.891854213354,4.));
#4959=CARTESIAN_POINT('',(141.784620240977,358.891854213354,4.));
#4960=CARTESIAN_POINT('',(63.,345.,4.));
#4961=CARTESIAN_POINT('',(-37.,335.,4.));
#4962=CARTESIAN_POINT('Origin',(0.,0.,-4.));
#4963=CARTESIAN_POINT('',(22.,329.539392014169,-4.));
#4964=CARTESIAN_POINT('Origin',(32.,329.539392014169,-4.));
#4965=CARTESIAN_POINT('',(22.,335.,-4.));
#4966=CARTESIAN_POINT('',(22.,335.,-4.));
#4967=CARTESIAN_POINT('',(11.842719282327,335.,-4.));
#4968=CARTESIAN_POINT('',(-37.,335.,-4.));
#4969=CARTESIAN_POINT('',(11.842719282327,335.,-4.));
#4970=CARTESIAN_POINT('',(141.784620240977,358.891854213354,-4.));
#4971=CARTESIAN_POINT('',(63.,345.,-4.));
#4972=CARTESIAN_POINT('',(143.521102017646,349.043776683232,-4.));
#4973=CARTESIAN_POINT('',(141.784620240977,358.891854213354,-4.));
#4974=CARTESIAN_POINT('',(63.8748866352591,335.,-4.));
#4975=CARTESIAN_POINT('',(64.7364817766693,335.151922469878,-4.));
#4976=CARTESIAN_POINT('',(-37.,335.,-4.));
#4977=CARTESIAN_POINT('',(-37.001,300.,-4.));
#4978=CARTESIAN_POINT('Origin',(-37.,335.,4.));
#4979=CARTESIAN_POINT('',(22.,335.,-25.2132034355964));
#4980=CARTESIAN_POINT('Origin',(0.,335.,0.));
#4981=CARTESIAN_POINT('Origin',(-37.,335.,4.));
#4982=CARTESIAN_POINT('',(63.8748866352591,335.,4.));
#4983=CARTESIAN_POINT('Origin',(64.7364817766693,335.151922469878,4.));
#4984=CARTESIAN_POINT('',(143.521102017646,349.043776683232,4.));
#4985=CARTESIAN_POINT('Origin',(141.784620240977,358.891854213354,4.));
#4986=CARTESIAN_POINT('',(141.784620240977,358.891854213354,4.));
#4987=CARTESIAN_POINT('Origin',(63.,345.,4.));
#4988=CARTESIAN_POINT('Origin',(0.,335.,0.));
#4989=CARTESIAN_POINT('Origin',(-37.001,300.,-4.));
#4990=CARTESIAN_POINT('Origin',(-37.001,300.,4.));
#4991=CARTESIAN_POINT('Origin',(22.,335.,-25.2132034355964));
#4992=CARTESIAN_POINT('',(22.,329.539392014169,4.));
#4993=CARTESIAN_POINT('Origin',(32.,329.539392014169,-25.2132034355964));
#4994=CARTESIAN_POINT('',(0.,0.,0.));
#4995=CARTESIAN_POINT('Origin',(-2.22044604925031E-15,50.1968749993855,
-2.77555756156289E-16));
#4996=CARTESIAN_POINT('',(-5.75643035625,62.0656249993855,-9.82515157185911E-16));
#4997=CARTESIAN_POINT('',(-5.75643035625,62.1781249993855,-9.82515157185911E-16));
#4998=CARTESIAN_POINT('',(-5.75643035625,50.1968749993855,-1.2600709133422E-15));
#4999=CARTESIAN_POINT('',(-2.878215178125,62.1406249993855,4.9852149236284));
#5000=CARTESIAN_POINT('Ctrl Pts',(-5.75643035625,62.0656249993855,-7.04959401029622E-16));
#5001=CARTESIAN_POINT('Ctrl Pts',(-5.75643035625,62.1031249993855,3.32347661575227));
#5002=CARTESIAN_POINT('Ctrl Pts',(-2.878215178125,62.1406249993855,4.9852149236284));
#5003=CARTESIAN_POINT('',(-2.878215178125,62.2531249993855,4.9852149236284));
#5004=CARTESIAN_POINT('',(-2.878215178125,62.1406249993855,4.9852149236284));
#5005=CARTESIAN_POINT('Ctrl Pts',(-5.75643035625,62.1781249993855,-7.04959401029622E-16));
#5006=CARTESIAN_POINT('Ctrl Pts',(-5.75643035625,62.2156249993855,3.32347661575227));
#5007=CARTESIAN_POINT('Ctrl Pts',(-2.878215178125,62.2531249993855,4.9852149236284));
#5008=CARTESIAN_POINT('Origin',(-2.22044604925031E-15,50.1968749993855,
-2.77555756156289E-16));
#5009=CARTESIAN_POINT('',(-5.75643035625,61.6156249993855,-9.82515157185911E-16));
#5010=CARTESIAN_POINT('',(-5.75643035625,61.7281249993855,-9.82515157185911E-16));
#5011=CARTESIAN_POINT('',(-5.75643035625,50.1968749993855,-1.2600709133422E-15));
#5012=CARTESIAN_POINT('Ctrl Pts',(-5.75643035625,61.6156249993855,-7.04959401029622E-16));
#5013=CARTESIAN_POINT('Ctrl Pts',(-5.75643035625,61.6531249993855,3.32347661575227));
#5014=CARTESIAN_POINT('Ctrl Pts',(-2.878215178125,61.6906249993855,4.9852149236284));
#5015=CARTESIAN_POINT('Ctrl Pts',(-1.22102549985663E-15,61.7281249993855,
6.64695323150454));
#5016=CARTESIAN_POINT('Ctrl Pts',(2.878215178125,61.7656249993855,4.98521492362841));
#5017=CARTESIAN_POINT('Ctrl Pts',(5.75643035625,61.8031249993855,3.32347661575227));
#5018=CARTESIAN_POINT('Ctrl Pts',(5.75643035625,61.8406249993855,0.));
#5019=CARTESIAN_POINT('Ctrl Pts',(5.75643035625,61.8781249993855,-3.32347661575227));
#5020=CARTESIAN_POINT('Ctrl Pts',(2.878215178125,61.9156249993855,-4.9852149236284));
#5021=CARTESIAN_POINT('Ctrl Pts',(4.0700849995221E-16,61.9531249993855,
-6.64695323150454));
#5022=CARTESIAN_POINT('Ctrl Pts',(-2.878215178125,61.9906249993855,-4.9852149236284));
#5023=CARTESIAN_POINT('Ctrl Pts',(-5.75643035625,62.0281249993855,-3.32347661575227));
#5024=CARTESIAN_POINT('Ctrl Pts',(-5.75643035625,62.0656249993855,-7.04959401029622E-16));
#5025=CARTESIAN_POINT('Ctrl Pts',(-5.75643035625,61.7281249993855,-7.04959401029622E-16));
#5026=CARTESIAN_POINT('Ctrl Pts',(-5.75643035625,61.7656249993855,3.32347661575227));
#5027=CARTESIAN_POINT('Ctrl Pts',(-2.878215178125,61.8031249993855,4.9852149236284));
#5028=CARTESIAN_POINT('Ctrl Pts',(-1.22102549985663E-15,61.8406249993855,
6.64695323150454));
#5029=CARTESIAN_POINT('Ctrl Pts',(2.878215178125,61.8781249993855,4.98521492362841));
#5030=CARTESIAN_POINT('Ctrl Pts',(5.75643035625,61.9156249993855,3.32347661575227));
#5031=CARTESIAN_POINT('Ctrl Pts',(5.75643035625,61.9531249993855,0.));
#5032=CARTESIAN_POINT('Ctrl Pts',(5.75643035625,61.9906249993855,-3.32347661575227));
#5033=CARTESIAN_POINT('Ctrl Pts',(2.878215178125,62.0281249993855,-4.9852149236284));
#5034=CARTESIAN_POINT('Ctrl Pts',(4.0700849995221E-16,62.0656249993855,
-6.64695323150454));
#5035=CARTESIAN_POINT('Ctrl Pts',(-2.878215178125,62.1031249993855,-4.9852149236284));
#5036=CARTESIAN_POINT('Ctrl Pts',(-5.75643035625,62.1406249993855,-3.32347661575227));
#5037=CARTESIAN_POINT('Ctrl Pts',(-5.75643035625,62.1781249993855,-7.04959401029622E-16));
#5038=CARTESIAN_POINT('Origin',(-2.22044604925031E-15,50.1968749993855,
-2.77555756156289E-16));
#5039=CARTESIAN_POINT('',(-5.75643035625,61.1656249993855,-9.82515157185911E-16));
#5040=CARTESIAN_POINT('',(-5.75643035625,61.2781249993855,-9.82515157185911E-16));
#5041=CARTESIAN_POINT('',(-5.75643035625,50.1968749993855,-1.2600709133422E-15));
#5042=CARTESIAN_POINT('Ctrl Pts',(-5.75643035625,61.1656249993855,-7.04959401029622E-16));
#5043=CARTESIAN_POINT('Ctrl Pts',(-5.75643035625,61.2031249993855,3.32347661575227));
#5044=CARTESIAN_POINT('Ctrl Pts',(-2.878215178125,61.2406249993855,4.9852149236284));
#5045=CARTESIAN_POINT('Ctrl Pts',(-1.22102549985663E-15,61.2781249993855,
6.64695323150454));
#5046=CARTESIAN_POINT('Ctrl Pts',(2.878215178125,61.3156249993855,4.98521492362841));
#5047=CARTESIAN_POINT('Ctrl Pts',(5.75643035625,61.3531249993855,3.32347661575227));
#5048=CARTESIAN_POINT('Ctrl Pts',(5.75643035625,61.3906249993855,0.));
#5049=CARTESIAN_POINT('Ctrl Pts',(5.75643035625,61.4281249993855,-3.32347661575227));
#5050=CARTESIAN_POINT('Ctrl Pts',(2.878215178125,61.4656249993855,-4.9852149236284));
#5051=CARTESIAN_POINT('Ctrl Pts',(4.0700849995221E-16,61.5031249993855,
-6.64695323150454));
#5052=CARTESIAN_POINT('Ctrl Pts',(-2.878215178125,61.5406249993855,-4.9852149236284));
#5053=CARTESIAN_POINT('Ctrl Pts',(-5.75643035625,61.5781249993855,-3.32347661575227));
#5054=CARTESIAN_POINT('Ctrl Pts',(-5.75643035625,61.6156249993855,-7.04959401029622E-16));
#5055=CARTESIAN_POINT('Ctrl Pts',(-5.75643035625,61.2781249993855,-7.04959401029622E-16));
#5056=CARTESIAN_POINT('Ctrl Pts',(-5.75643035625,61.3156249993855,3.32347661575227));
#5057=CARTESIAN_POINT('Ctrl Pts',(-2.878215178125,61.3531249993855,4.9852149236284));
#5058=CARTESIAN_POINT('Ctrl Pts',(-1.22102549985663E-15,61.3906249993855,
6.64695323150454));
#5059=CARTESIAN_POINT('Ctrl Pts',(2.878215178125,61.4281249993855,4.98521492362841));
#5060=CARTESIAN_POINT('Ctrl Pts',(5.75643035625,61.4656249993855,3.32347661575227));
#5061=CARTESIAN_POINT('Ctrl Pts',(5.75643035625,61.5031249993855,0.));
#5062=CARTESIAN_POINT('Ctrl Pts',(5.75643035625,61.5406249993855,-3.32347661575227));
#5063=CARTESIAN_POINT('Ctrl Pts',(2.878215178125,61.5781249993855,-4.9852149236284));
#5064=CARTESIAN_POINT('Ctrl Pts',(4.0700849995221E-16,61.6156249993855,
-6.64695323150454));
#5065=CARTESIAN_POINT('Ctrl Pts',(-2.878215178125,61.6531249993855,-4.9852149236284));
#5066=CARTESIAN_POINT('Ctrl Pts',(-5.75643035625,61.6906249993855,-3.32347661575227));
#5067=CARTESIAN_POINT('Ctrl Pts',(-5.75643035625,61.7281249993855,-7.04959401029622E-16));
#5068=CARTESIAN_POINT('Origin',(-2.22044604925031E-15,50.1968749993855,
-2.77555756156289E-16));
#5069=CARTESIAN_POINT('',(-5.75643035625,60.7156249993855,-9.82515157185911E-16));
#5070=CARTESIAN_POINT('',(-5.75643035625,60.8281249993855,-9.82515157185911E-16));
#5071=CARTESIAN_POINT('',(-5.75643035625,50.1968749993855,-1.2600709133422E-15));
#5072=CARTESIAN_POINT('Ctrl Pts',(-5.75643035625,60.7156249993855,-7.04959401029622E-16));
#5073=CARTESIAN_POINT('Ctrl Pts',(-5.75643035625,60.7531249993855,3.32347661575227));
#5074=CARTESIAN_POINT('Ctrl Pts',(-2.878215178125,60.7906249993855,4.9852149236284));
#5075=CARTESIAN_POINT('Ctrl Pts',(-1.22102549985663E-15,60.8281249993855,
6.64695323150454));
#5076=CARTESIAN_POINT('Ctrl Pts',(2.878215178125,60.8656249993855,4.98521492362841));
#5077=CARTESIAN_POINT('Ctrl Pts',(5.75643035625,60.9031249993855,3.32347661575227));
#5078=CARTESIAN_POINT('Ctrl Pts',(5.75643035625,60.9406249993855,0.));
#5079=CARTESIAN_POINT('Ctrl Pts',(5.75643035625,60.9781249993855,-3.32347661575227));
#5080=CARTESIAN_POINT('Ctrl Pts',(2.878215178125,61.0156249993855,-4.9852149236284));
#5081=CARTESIAN_POINT('Ctrl Pts',(4.0700849995221E-16,61.0531249993855,
-6.64695323150454));
#5082=CARTESIAN_POINT('Ctrl Pts',(-2.878215178125,61.0906249993855,-4.9852149236284));
#5083=CARTESIAN_POINT('Ctrl Pts',(-5.75643035625,61.1281249993855,-3.32347661575227));
#5084=CARTESIAN_POINT('Ctrl Pts',(-5.75643035625,61.1656249993855,-7.04959401029622E-16));
#5085=CARTESIAN_POINT('Ctrl Pts',(-5.75643035625,60.8281249993855,-7.04959401029622E-16));
#5086=CARTESIAN_POINT('Ctrl Pts',(-5.75643035625,60.8656249993855,3.32347661575227));
#5087=CARTESIAN_POINT('Ctrl Pts',(-2.878215178125,60.9031249993855,4.9852149236284));
#5088=CARTESIAN_POINT('Ctrl Pts',(-1.22102549985663E-15,60.9406249993855,
6.64695323150454));
#5089=CARTESIAN_POINT('Ctrl Pts',(2.878215178125,60.9781249993855,4.98521492362841));
#5090=CARTESIAN_POINT('Ctrl Pts',(5.75643035625,61.0156249993855,3.32347661575227));
#5091=CARTESIAN_POINT('Ctrl Pts',(5.75643035625,61.0531249993855,0.));
#5092=CARTESIAN_POINT('Ctrl Pts',(5.75643035625,61.0906249993855,-3.32347661575227));
#5093=CARTESIAN_POINT('Ctrl Pts',(2.878215178125,61.1281249993855,-4.9852149236284));
#5094=CARTESIAN_POINT('Ctrl Pts',(4.0700849995221E-16,61.1656249993855,
-6.64695323150454));
#5095=CARTESIAN_POINT('Ctrl Pts',(-2.878215178125,61.2031249993855,-4.9852149236284));
#5096=CARTESIAN_POINT('Ctrl Pts',(-5.75643035625,61.2406249993855,-3.32347661575227));
#5097=CARTESIAN_POINT('Ctrl Pts',(-5.75643035625,61.2781249993855,-7.04959401029622E-16));
#5098=CARTESIAN_POINT('Origin',(-2.22044604925031E-15,50.1968749993855,
-2.77555756156289E-16));
#5099=CARTESIAN_POINT('',(-5.75643035625,60.2656249993855,-9.82515157185911E-16));
#5100=CARTESIAN_POINT('',(-5.75643035625,60.3781249993855,-9.82515157185911E-16));
#5101=CARTESIAN_POINT('',(-5.75643035625,50.1968749993855,-1.2600709133422E-15));
#5102=CARTESIAN_POINT('Ctrl Pts',(-5.75643035625,60.2656249993855,-7.04959401029622E-16));
#5103=CARTESIAN_POINT('Ctrl Pts',(-5.75643035625,60.3031249993855,3.32347661575227));
#5104=CARTESIAN_POINT('Ctrl Pts',(-2.878215178125,60.3406249993855,4.9852149236284));
#5105=CARTESIAN_POINT('Ctrl Pts',(-1.22102549985663E-15,60.3781249993855,
6.64695323150454));
#5106=CARTESIAN_POINT('Ctrl Pts',(2.878215178125,60.4156249993855,4.98521492362841));
#5107=CARTESIAN_POINT('Ctrl Pts',(5.75643035625,60.4531249993855,3.32347661575227));
#5108=CARTESIAN_POINT('Ctrl Pts',(5.75643035625,60.4906249993855,0.));
#5109=CARTESIAN_POINT('Ctrl Pts',(5.75643035625,60.5281249993855,-3.32347661575227));
#5110=CARTESIAN_POINT('Ctrl Pts',(2.878215178125,60.5656249993855,-4.9852149236284));
#5111=CARTESIAN_POINT('Ctrl Pts',(4.0700849995221E-16,60.6031249993855,
-6.64695323150454));
#5112=CARTESIAN_POINT('Ctrl Pts',(-2.878215178125,60.6406249993855,-4.9852149236284));
#5113=CARTESIAN_POINT('Ctrl Pts',(-5.75643035625,60.6781249993855,-3.32347661575227));
#5114=CARTESIAN_POINT('Ctrl Pts',(-5.75643035625,60.7156249993855,-7.04959401029622E-16));
#5115=CARTESIAN_POINT('Ctrl Pts',(-5.75643035625,60.3781249993855,-7.04959401029622E-16));
#5116=CARTESIAN_POINT('Ctrl Pts',(-5.75643035625,60.4156249993855,3.32347661575227));
#5117=CARTESIAN_POINT('Ctrl Pts',(-2.878215178125,60.4531249993855,4.9852149236284));
#5118=CARTESIAN_POINT('Ctrl Pts',(-1.22102549985663E-15,60.4906249993855,
6.64695323150454));
#5119=CARTESIAN_POINT('Ctrl Pts',(2.878215178125,60.5281249993855,4.98521492362841));
#5120=CARTESIAN_POINT('Ctrl Pts',(5.75643035625,60.5656249993855,3.32347661575227));
#5121=CARTESIAN_POINT('Ctrl Pts',(5.75643035625,60.6031249993855,0.));
#5122=CARTESIAN_POINT('Ctrl Pts',(5.75643035625,60.6406249993855,-3.32347661575227));
#5123=CARTESIAN_POINT('Ctrl Pts',(2.878215178125,60.6781249993855,-4.9852149236284));
#5124=CARTESIAN_POINT('Ctrl Pts',(4.0700849995221E-16,60.7156249993855,
-6.64695323150454));
#5125=CARTESIAN_POINT('Ctrl Pts',(-2.878215178125,60.7531249993855,-4.9852149236284));
#5126=CARTESIAN_POINT('Ctrl Pts',(-5.75643035625,60.7906249993855,-3.32347661575227));
#5127=CARTESIAN_POINT('Ctrl Pts',(-5.75643035625,60.8281249993855,-7.04959401029622E-16));
#5128=CARTESIAN_POINT('Origin',(-2.22044604925031E-15,50.1968749993855,
-2.77555756156289E-16));
#5129=CARTESIAN_POINT('',(-5.75643035625,59.8156249993855,-9.82515157185911E-16));
#5130=CARTESIAN_POINT('',(-5.75643035625,59.9281249993855,-9.82515157185911E-16));
#5131=CARTESIAN_POINT('',(-5.75643035625,50.1968749993855,-1.2600709133422E-15));
#5132=CARTESIAN_POINT('Ctrl Pts',(-5.75643035625,59.8156249993855,-7.04959401029622E-16));
#5133=CARTESIAN_POINT('Ctrl Pts',(-5.75643035625,59.8531249993855,3.32347661575227));
#5134=CARTESIAN_POINT('Ctrl Pts',(-2.878215178125,59.8906249993855,4.9852149236284));
#5135=CARTESIAN_POINT('Ctrl Pts',(-1.22102549985663E-15,59.9281249993855,
6.64695323150454));
#5136=CARTESIAN_POINT('Ctrl Pts',(2.878215178125,59.9656249993855,4.98521492362841));
#5137=CARTESIAN_POINT('Ctrl Pts',(5.75643035625,60.0031249993855,3.32347661575227));
#5138=CARTESIAN_POINT('Ctrl Pts',(5.75643035625,60.0406249993855,0.));
#5139=CARTESIAN_POINT('Ctrl Pts',(5.75643035625,60.0781249993855,-3.32347661575227));
#5140=CARTESIAN_POINT('Ctrl Pts',(2.878215178125,60.1156249993855,-4.9852149236284));
#5141=CARTESIAN_POINT('Ctrl Pts',(4.0700849995221E-16,60.1531249993855,
-6.64695323150454));
#5142=CARTESIAN_POINT('Ctrl Pts',(-2.878215178125,60.1906249993855,-4.9852149236284));
#5143=CARTESIAN_POINT('Ctrl Pts',(-5.75643035625,60.2281249993855,-3.32347661575227));
#5144=CARTESIAN_POINT('Ctrl Pts',(-5.75643035625,60.2656249993855,-7.04959401029622E-16));
#5145=CARTESIAN_POINT('Ctrl Pts',(-5.75643035625,59.9281249993855,-7.04959401029622E-16));
#5146=CARTESIAN_POINT('Ctrl Pts',(-5.75643035625,59.9656249993855,3.32347661575227));
#5147=CARTESIAN_POINT('Ctrl Pts',(-2.878215178125,60.0031249993855,4.9852149236284));
#5148=CARTESIAN_POINT('Ctrl Pts',(-1.22102549985663E-15,60.0406249993855,
6.64695323150454));
#5149=CARTESIAN_POINT('Ctrl Pts',(2.878215178125,60.0781249993855,4.98521492362841));
#5150=CARTESIAN_POINT('Ctrl Pts',(5.75643035625,60.1156249993855,3.32347661575227));
#5151=CARTESIAN_POINT('Ctrl Pts',(5.75643035625,60.1531249993855,0.));
#5152=CARTESIAN_POINT('Ctrl Pts',(5.75643035625,60.1906249993855,-3.32347661575227));
#5153=CARTESIAN_POINT('Ctrl Pts',(2.878215178125,60.2281249993855,-4.9852149236284));
#5154=CARTESIAN_POINT('Ctrl Pts',(4.0700849995221E-16,60.2656249993855,
-6.64695323150454));
#5155=CARTESIAN_POINT('Ctrl Pts',(-2.878215178125,60.3031249993855,-4.9852149236284));
#5156=CARTESIAN_POINT('Ctrl Pts',(-5.75643035625,60.3406249993855,-3.32347661575227));
#5157=CARTESIAN_POINT('Ctrl Pts',(-5.75643035625,60.3781249993855,-7.04959401029622E-16));
#5158=CARTESIAN_POINT('Origin',(-2.22044604925031E-15,50.1968749993855,
-2.77555756156289E-16));
#5159=CARTESIAN_POINT('',(-5.75643035625,59.3656249993855,-9.82515157185911E-16));
#5160=CARTESIAN_POINT('',(-5.75643035625,59.4781249993855,-9.82515157185911E-16));
#5161=CARTESIAN_POINT('',(-5.75643035625,50.1968749993855,-1.2600709133422E-15));
#5162=CARTESIAN_POINT('Ctrl Pts',(-5.75643035625,59.3656249993855,-7.04959401029622E-16));
#5163=CARTESIAN_POINT('Ctrl Pts',(-5.75643035625,59.4031249993855,3.32347661575227));
#5164=CARTESIAN_POINT('Ctrl Pts',(-2.878215178125,59.4406249993855,4.9852149236284));
#5165=CARTESIAN_POINT('Ctrl Pts',(-1.22102549985663E-15,59.4781249993855,
6.64695323150454));
#5166=CARTESIAN_POINT('Ctrl Pts',(2.878215178125,59.5156249993855,4.98521492362841));
#5167=CARTESIAN_POINT('Ctrl Pts',(5.75643035625,59.5531249993855,3.32347661575227));
#5168=CARTESIAN_POINT('Ctrl Pts',(5.75643035625,59.5906249993855,0.));
#5169=CARTESIAN_POINT('Ctrl Pts',(5.75643035625,59.6281249993855,-3.32347661575227));
#5170=CARTESIAN_POINT('Ctrl Pts',(2.878215178125,59.6656249993855,-4.9852149236284));
#5171=CARTESIAN_POINT('Ctrl Pts',(4.0700849995221E-16,59.7031249993855,
-6.64695323150454));
#5172=CARTESIAN_POINT('Ctrl Pts',(-2.878215178125,59.7406249993855,-4.9852149236284));
#5173=CARTESIAN_POINT('Ctrl Pts',(-5.75643035625,59.7781249993855,-3.32347661575227));
#5174=CARTESIAN_POINT('Ctrl Pts',(-5.75643035625,59.8156249993855,-7.04959401029622E-16));
#5175=CARTESIAN_POINT('Ctrl Pts',(-5.75643035625,59.4781249993855,-7.04959401029622E-16));
#5176=CARTESIAN_POINT('Ctrl Pts',(-5.75643035625,59.5156249993855,3.32347661575227));
#5177=CARTESIAN_POINT('Ctrl Pts',(-2.878215178125,59.5531249993855,4.9852149236284));
#5178=CARTESIAN_POINT('Ctrl Pts',(-1.22102549985663E-15,59.5906249993855,
6.64695323150454));
#5179=CARTESIAN_POINT('Ctrl Pts',(2.878215178125,59.6281249993855,4.98521492362841));
#5180=CARTESIAN_POINT('Ctrl Pts',(5.75643035625,59.6656249993855,3.32347661575227));
#5181=CARTESIAN_POINT('Ctrl Pts',(5.75643035625,59.7031249993855,0.));
#5182=CARTESIAN_POINT('Ctrl Pts',(5.75643035625,59.7406249993855,-3.32347661575227));
#5183=CARTESIAN_POINT('Ctrl Pts',(2.878215178125,59.7781249993855,-4.9852149236284));
#5184=CARTESIAN_POINT('Ctrl Pts',(4.0700849995221E-16,59.8156249993855,
-6.64695323150454));
#5185=CARTESIAN_POINT('Ctrl Pts',(-2.878215178125,59.8531249993855,-4.9852149236284));
#5186=CARTESIAN_POINT('Ctrl Pts',(-5.75643035625,59.8906249993855,-3.32347661575227));
#5187=CARTESIAN_POINT('Ctrl Pts',(-5.75643035625,59.9281249993855,-7.04959401029622E-16));
#5188=CARTESIAN_POINT('Origin',(-2.22044604925031E-15,50.1968749993855,
-2.77555756156289E-16));
#5189=CARTESIAN_POINT('',(-5.75643035625,58.9156249993855,-9.82515157185911E-16));
#5190=CARTESIAN_POINT('',(-5.75643035625,59.0281249993855,-9.82515157185911E-16));
#5191=CARTESIAN_POINT('',(-5.75643035625,50.1968749993855,-1.2600709133422E-15));
#5192=CARTESIAN_POINT('Ctrl Pts',(-5.75643035625,58.9156249993855,-7.04959401029622E-16));
#5193=CARTESIAN_POINT('Ctrl Pts',(-5.75643035625,58.9531249993855,3.32347661575227));
#5194=CARTESIAN_POINT('Ctrl Pts',(-2.878215178125,58.9906249993855,4.9852149236284));
#5195=CARTESIAN_POINT('Ctrl Pts',(-1.22102549985663E-15,59.0281249993855,
6.64695323150454));
#5196=CARTESIAN_POINT('Ctrl Pts',(2.878215178125,59.0656249993855,4.98521492362841));
#5197=CARTESIAN_POINT('Ctrl Pts',(5.75643035625,59.1031249993855,3.32347661575227));
#5198=CARTESIAN_POINT('Ctrl Pts',(5.75643035625,59.1406249993855,0.));
#5199=CARTESIAN_POINT('Ctrl Pts',(5.75643035625,59.1781249993855,-3.32347661575227));
#5200=CARTESIAN_POINT('Ctrl Pts',(2.878215178125,59.2156249993855,-4.9852149236284));
#5201=CARTESIAN_POINT('Ctrl Pts',(4.0700849995221E-16,59.2531249993855,
-6.64695323150454));
#5202=CARTESIAN_POINT('Ctrl Pts',(-2.878215178125,59.2906249993855,-4.9852149236284));
#5203=CARTESIAN_POINT('Ctrl Pts',(-5.75643035625,59.3281249993855,-3.32347661575227));
#5204=CARTESIAN_POINT('Ctrl Pts',(-5.75643035625,59.3656249993855,-7.04959401029622E-16));
#5205=CARTESIAN_POINT('Ctrl Pts',(-5.75643035625,59.0281249993855,-7.04959401029622E-16));
#5206=CARTESIAN_POINT('Ctrl Pts',(-5.75643035625,59.0656249993855,3.32347661575227));
#5207=CARTESIAN_POINT('Ctrl Pts',(-2.878215178125,59.1031249993855,4.9852149236284));
#5208=CARTESIAN_POINT('Ctrl Pts',(-1.22102549985663E-15,59.1406249993855,
6.64695323150454));
#5209=CARTESIAN_POINT('Ctrl Pts',(2.878215178125,59.1781249993855,4.98521492362841));
#5210=CARTESIAN_POINT('Ctrl Pts',(5.75643035625,59.2156249993855,3.32347661575227));
#5211=CARTESIAN_POINT('Ctrl Pts',(5.75643035625,59.2531249993855,0.));
#5212=CARTESIAN_POINT('Ctrl Pts',(5.75643035625,59.2906249993855,-3.32347661575227));
#5213=CARTESIAN_POINT('Ctrl Pts',(2.878215178125,59.3281249993855,-4.9852149236284));
#5214=CARTESIAN_POINT('Ctrl Pts',(4.0700849995221E-16,59.3656249993855,
-6.64695323150454));
#5215=CARTESIAN_POINT('Ctrl Pts',(-2.878215178125,59.4031249993855,-4.9852149236284));
#5216=CARTESIAN_POINT('Ctrl Pts',(-5.75643035625,59.4406249993855,-3.32347661575227));
#5217=CARTESIAN_POINT('Ctrl Pts',(-5.75643035625,59.4781249993855,-7.04959401029622E-16));
#5218=CARTESIAN_POINT('Origin',(-2.22044604925031E-15,50.1968749993855,
-2.77555756156289E-16));
#5219=CARTESIAN_POINT('',(-5.75643035625,58.4656249993855,-9.82515157185911E-16));
#5220=CARTESIAN_POINT('',(-5.75643035625,58.5781249993855,-9.82515157185911E-16));
#5221=CARTESIAN_POINT('',(-5.75643035625,50.1968749993855,-1.2600709133422E-15));
#5222=CARTESIAN_POINT('Ctrl Pts',(-5.75643035625,58.4656249993855,-7.04959401029622E-16));
#5223=CARTESIAN_POINT('Ctrl Pts',(-5.75643035625,58.5031249993855,3.32347661575227));
#5224=CARTESIAN_POINT('Ctrl Pts',(-2.878215178125,58.5406249993855,4.9852149236284));
#5225=CARTESIAN_POINT('Ctrl Pts',(-1.22102549985663E-15,58.5781249993855,
6.64695323150454));
#5226=CARTESIAN_POINT('Ctrl Pts',(2.878215178125,58.6156249993855,4.98521492362841));
#5227=CARTESIAN_POINT('Ctrl Pts',(5.75643035625,58.6531249993855,3.32347661575227));
#5228=CARTESIAN_POINT('Ctrl Pts',(5.75643035625,58.6906249993855,0.));
#5229=CARTESIAN_POINT('Ctrl Pts',(5.75643035625,58.7281249993855,-3.32347661575227));
#5230=CARTESIAN_POINT('Ctrl Pts',(2.878215178125,58.7656249993855,-4.9852149236284));
#5231=CARTESIAN_POINT('Ctrl Pts',(4.0700849995221E-16,58.8031249993855,
-6.64695323150454));
#5232=CARTESIAN_POINT('Ctrl Pts',(-2.878215178125,58.8406249993855,-4.9852149236284));
#5233=CARTESIAN_POINT('Ctrl Pts',(-5.75643035625,58.8781249993855,-3.32347661575227));
#5234=CARTESIAN_POINT('Ctrl Pts',(-5.75643035625,58.9156249993855,-7.04959401029622E-16));
#5235=CARTESIAN_POINT('Ctrl Pts',(-5.75643035625,58.5781249993855,-7.04959401029622E-16));
#5236=CARTESIAN_POINT('Ctrl Pts',(-5.75643035625,58.6156249993855,3.32347661575227));
#5237=CARTESIAN_POINT('Ctrl Pts',(-2.878215178125,58.6531249993855,4.9852149236284));
#5238=CARTESIAN_POINT('Ctrl Pts',(-1.22102549985663E-15,58.6906249993855,
6.64695323150454));
#5239=CARTESIAN_POINT('Ctrl Pts',(2.878215178125,58.7281249993855,4.98521492362841));
#5240=CARTESIAN_POINT('Ctrl Pts',(5.75643035625,58.7656249993855,3.32347661575227));
#5241=CARTESIAN_POINT('Ctrl Pts',(5.75643035625,58.8031249993855,0.));
#5242=CARTESIAN_POINT('Ctrl Pts',(5.75643035625,58.8406249993855,-3.32347661575227));
#5243=CARTESIAN_POINT('Ctrl Pts',(2.878215178125,58.8781249993855,-4.9852149236284));
#5244=CARTESIAN_POINT('Ctrl Pts',(4.0700849995221E-16,58.9156249993855,
-6.64695323150454));
#5245=CARTESIAN_POINT('Ctrl Pts',(-2.878215178125,58.9531249993855,-4.9852149236284));
#5246=CARTESIAN_POINT('Ctrl Pts',(-5.75643035625,58.9906249993855,-3.32347661575227));
#5247=CARTESIAN_POINT('Ctrl Pts',(-5.75643035625,59.0281249993855,-7.04959401029622E-16));
#5248=CARTESIAN_POINT('Origin',(-2.22044604925031E-15,50.1968749993855,
-2.77555756156289E-16));
#5249=CARTESIAN_POINT('',(-5.75643035625,58.0156249993855,-9.82515157185911E-16));
#5250=CARTESIAN_POINT('',(-5.75643035625,58.1281249993855,-9.82515157185911E-16));
#5251=CARTESIAN_POINT('',(-5.75643035625,50.1968749993855,-1.2600709133422E-15));
#5252=CARTESIAN_POINT('Ctrl Pts',(-5.75643035625,58.0156249993855,-7.04959401029622E-16));
#5253=CARTESIAN_POINT('Ctrl Pts',(-5.75643035625,58.0531249993855,3.32347661575227));
#5254=CARTESIAN_POINT('Ctrl Pts',(-2.878215178125,58.0906249993855,4.9852149236284));
#5255=CARTESIAN_POINT('Ctrl Pts',(-1.22102549985663E-15,58.1281249993855,
6.64695323150454));
#5256=CARTESIAN_POINT('Ctrl Pts',(2.878215178125,58.1656249993855,4.98521492362841));
#5257=CARTESIAN_POINT('Ctrl Pts',(5.75643035625,58.2031249993855,3.32347661575227));
#5258=CARTESIAN_POINT('Ctrl Pts',(5.75643035625,58.2406249993855,0.));
#5259=CARTESIAN_POINT('Ctrl Pts',(5.75643035625,58.2781249993855,-3.32347661575227));
#5260=CARTESIAN_POINT('Ctrl Pts',(2.878215178125,58.3156249993855,-4.9852149236284));
#5261=CARTESIAN_POINT('Ctrl Pts',(4.0700849995221E-16,58.3531249993855,
-6.64695323150454));
#5262=CARTESIAN_POINT('Ctrl Pts',(-2.878215178125,58.3906249993855,-4.9852149236284));
#5263=CARTESIAN_POINT('Ctrl Pts',(-5.75643035625,58.4281249993855,-3.32347661575227));
#5264=CARTESIAN_POINT('Ctrl Pts',(-5.75643035625,58.4656249993855,-7.04959401029622E-16));
#5265=CARTESIAN_POINT('Ctrl Pts',(-5.75643035625,58.1281249993855,-7.04959401029622E-16));
#5266=CARTESIAN_POINT('Ctrl Pts',(-5.75643035625,58.1656249993855,3.32347661575227));
#5267=CARTESIAN_POINT('Ctrl Pts',(-2.878215178125,58.2031249993855,4.9852149236284));
#5268=CARTESIAN_POINT('Ctrl Pts',(-1.22102549985663E-15,58.2406249993855,
6.64695323150454));
#5269=CARTESIAN_POINT('Ctrl Pts',(2.878215178125,58.2781249993855,4.98521492362841));
#5270=CARTESIAN_POINT('Ctrl Pts',(5.75643035625,58.3156249993855,3.32347661575227));
#5271=CARTESIAN_POINT('Ctrl Pts',(5.75643035625,58.3531249993855,0.));
#5272=CARTESIAN_POINT('Ctrl Pts',(5.75643035625,58.3906249993855,-3.32347661575227));
#5273=CARTESIAN_POINT('Ctrl Pts',(2.878215178125,58.4281249993855,-4.9852149236284));
#5274=CARTESIAN_POINT('Ctrl Pts',(4.0700849995221E-16,58.4656249993855,
-6.64695323150454));
#5275=CARTESIAN_POINT('Ctrl Pts',(-2.878215178125,58.5031249993855,-4.9852149236284));
#5276=CARTESIAN_POINT('Ctrl Pts',(-5.75643035625,58.5406249993855,-3.32347661575227));
#5277=CARTESIAN_POINT('Ctrl Pts',(-5.75643035625,58.5781249993855,-7.04959401029622E-16));
#5278=CARTESIAN_POINT('Origin',(-2.22044604925031E-15,50.1968749993855,
-2.77555756156289E-16));
#5279=CARTESIAN_POINT('',(-5.75643035625,57.5656249993855,-9.82515157185911E-16));
#5280=CARTESIAN_POINT('',(-5.75643035625,57.6781249993855,-9.82515157185911E-16));
#5281=CARTESIAN_POINT('',(-5.75643035625,50.1968749993855,-1.2600709133422E-15));
#5282=CARTESIAN_POINT('Ctrl Pts',(-5.75643035625,57.5656249993855,-7.04959401029622E-16));
#5283=CARTESIAN_POINT('Ctrl Pts',(-5.75643035625,57.6031249993855,3.32347661575227));
#5284=CARTESIAN_POINT('Ctrl Pts',(-2.878215178125,57.6406249993855,4.9852149236284));
#5285=CARTESIAN_POINT('Ctrl Pts',(-1.22102549985663E-15,57.6781249993855,
6.64695323150454));
#5286=CARTESIAN_POINT('Ctrl Pts',(2.878215178125,57.7156249993855,4.98521492362841));
#5287=CARTESIAN_POINT('Ctrl Pts',(5.75643035625,57.7531249993855,3.32347661575227));
#5288=CARTESIAN_POINT('Ctrl Pts',(5.75643035625,57.7906249993855,0.));
#5289=CARTESIAN_POINT('Ctrl Pts',(5.75643035625,57.8281249993855,-3.32347661575227));
#5290=CARTESIAN_POINT('Ctrl Pts',(2.878215178125,57.8656249993855,-4.9852149236284));
#5291=CARTESIAN_POINT('Ctrl Pts',(4.0700849995221E-16,57.9031249993855,
-6.64695323150454));
#5292=CARTESIAN_POINT('Ctrl Pts',(-2.878215178125,57.9406249993855,-4.9852149236284));
#5293=CARTESIAN_POINT('Ctrl Pts',(-5.75643035625,57.9781249993855,-3.32347661575227));
#5294=CARTESIAN_POINT('Ctrl Pts',(-5.75643035625,58.0156249993855,-7.04959401029622E-16));
#5295=CARTESIAN_POINT('Ctrl Pts',(-5.75643035625,57.6781249993855,-7.04959401029622E-16));
#5296=CARTESIAN_POINT('Ctrl Pts',(-5.75643035625,57.7156249993855,3.32347661575227));
#5297=CARTESIAN_POINT('Ctrl Pts',(-2.878215178125,57.7531249993855,4.9852149236284));
#5298=CARTESIAN_POINT('Ctrl Pts',(-1.22102549985663E-15,57.7906249993855,
6.64695323150454));
#5299=CARTESIAN_POINT('Ctrl Pts',(2.878215178125,57.8281249993855,4.98521492362841));
#5300=CARTESIAN_POINT('Ctrl Pts',(5.75643035625,57.8656249993855,3.32347661575227));
#5301=CARTESIAN_POINT('Ctrl Pts',(5.75643035625,57.9031249993855,0.));
#5302=CARTESIAN_POINT('Ctrl Pts',(5.75643035625,57.9406249993855,-3.32347661575227));
#5303=CARTESIAN_POINT('Ctrl Pts',(2.878215178125,57.9781249993855,-4.9852149236284));
#5304=CARTESIAN_POINT('Ctrl Pts',(4.0700849995221E-16,58.0156249993855,
-6.64695323150454));
#5305=CARTESIAN_POINT('Ctrl Pts',(-2.878215178125,58.0531249993855,-4.9852149236284));
#5306=CARTESIAN_POINT('Ctrl Pts',(-5.75643035625,58.0906249993855,-3.32347661575227));
#5307=CARTESIAN_POINT('Ctrl Pts',(-5.75643035625,58.1281249993855,-7.04959401029622E-16));
#5308=CARTESIAN_POINT('Origin',(-2.22044604925031E-15,50.1968749993855,
-2.77555756156289E-16));
#5309=CARTESIAN_POINT('',(-5.75643035625,57.1156249993855,-9.82515157185911E-16));
#5310=CARTESIAN_POINT('',(-5.75643035625,57.2281249993855,-9.82515157185911E-16));
#5311=CARTESIAN_POINT('',(-5.75643035625,50.1968749993855,-1.2600709133422E-15));
#5312=CARTESIAN_POINT('Ctrl Pts',(-5.75643035625,57.1156249993855,-7.04959401029622E-16));
#5313=CARTESIAN_POINT('Ctrl Pts',(-5.75643035625,57.1531249993855,3.32347661575227));
#5314=CARTESIAN_POINT('Ctrl Pts',(-2.878215178125,57.1906249993855,4.9852149236284));
#5315=CARTESIAN_POINT('Ctrl Pts',(-1.22102549985663E-15,57.2281249993855,
6.64695323150454));
#5316=CARTESIAN_POINT('Ctrl Pts',(2.878215178125,57.2656249993855,4.98521492362841));
#5317=CARTESIAN_POINT('Ctrl Pts',(5.75643035625,57.3031249993855,3.32347661575227));
#5318=CARTESIAN_POINT('Ctrl Pts',(5.75643035625,57.3406249993855,0.));
#5319=CARTESIAN_POINT('Ctrl Pts',(5.75643035625,57.3781249993855,-3.32347661575227));
#5320=CARTESIAN_POINT('Ctrl Pts',(2.878215178125,57.4156249993855,-4.9852149236284));
#5321=CARTESIAN_POINT('Ctrl Pts',(4.0700849995221E-16,57.4531249993855,
-6.64695323150454));
#5322=CARTESIAN_POINT('Ctrl Pts',(-2.878215178125,57.4906249993855,-4.9852149236284));
#5323=CARTESIAN_POINT('Ctrl Pts',(-5.75643035625,57.5281249993855,-3.32347661575227));
#5324=CARTESIAN_POINT('Ctrl Pts',(-5.75643035625,57.5656249993855,-7.04959401029622E-16));
#5325=CARTESIAN_POINT('Ctrl Pts',(-5.75643035625,57.2281249993855,-7.04959401029622E-16));
#5326=CARTESIAN_POINT('Ctrl Pts',(-5.75643035625,57.2656249993855,3.32347661575227));
#5327=CARTESIAN_POINT('Ctrl Pts',(-2.878215178125,57.3031249993855,4.9852149236284));
#5328=CARTESIAN_POINT('Ctrl Pts',(-1.22102549985663E-15,57.3406249993855,
6.64695323150454));
#5329=CARTESIAN_POINT('Ctrl Pts',(2.878215178125,57.3781249993855,4.98521492362841));
#5330=CARTESIAN_POINT('Ctrl Pts',(5.75643035625,57.4156249993855,3.32347661575227));
#5331=CARTESIAN_POINT('Ctrl Pts',(5.75643035625,57.4531249993855,0.));
#5332=CARTESIAN_POINT('Ctrl Pts',(5.75643035625,57.4906249993855,-3.32347661575227));
#5333=CARTESIAN_POINT('Ctrl Pts',(2.878215178125,57.5281249993855,-4.9852149236284));
#5334=CARTESIAN_POINT('Ctrl Pts',(4.0700849995221E-16,57.5656249993855,
-6.64695323150454));
#5335=CARTESIAN_POINT('Ctrl Pts',(-2.878215178125,57.6031249993855,-4.9852149236284));
#5336=CARTESIAN_POINT('Ctrl Pts',(-5.75643035625,57.6406249993855,-3.32347661575227));
#5337=CARTESIAN_POINT('Ctrl Pts',(-5.75643035625,57.6781249993855,-7.04959401029622E-16));
#5338=CARTESIAN_POINT('Origin',(-2.22044604925031E-15,50.1968749993855,
-2.77555756156289E-16));
#5339=CARTESIAN_POINT('',(-5.75643035625,56.6656249993855,-9.82515157185911E-16));
#5340=CARTESIAN_POINT('',(-5.75643035625,56.7781249993855,-9.82515157185911E-16));
#5341=CARTESIAN_POINT('',(-5.75643035625,50.1968749993855,-1.2600709133422E-15));
#5342=CARTESIAN_POINT('Ctrl Pts',(-5.75643035625,56.6656249993855,-7.04959401029622E-16));
#5343=CARTESIAN_POINT('Ctrl Pts',(-5.75643035625,56.7031249993855,3.32347661575227));
#5344=CARTESIAN_POINT('Ctrl Pts',(-2.878215178125,56.7406249993855,4.9852149236284));
#5345=CARTESIAN_POINT('Ctrl Pts',(-1.22102549985663E-15,56.7781249993855,
6.64695323150454));
#5346=CARTESIAN_POINT('Ctrl Pts',(2.878215178125,56.8156249993855,4.98521492362841));
#5347=CARTESIAN_POINT('Ctrl Pts',(5.75643035625,56.8531249993855,3.32347661575227));
#5348=CARTESIAN_POINT('Ctrl Pts',(5.75643035625,56.8906249993855,0.));
#5349=CARTESIAN_POINT('Ctrl Pts',(5.75643035625,56.9281249993855,-3.32347661575227));
#5350=CARTESIAN_POINT('Ctrl Pts',(2.878215178125,56.9656249993855,-4.9852149236284));
#5351=CARTESIAN_POINT('Ctrl Pts',(4.0700849995221E-16,57.0031249993855,
-6.64695323150454));
#5352=CARTESIAN_POINT('Ctrl Pts',(-2.878215178125,57.0406249993855,-4.9852149236284));
#5353=CARTESIAN_POINT('Ctrl Pts',(-5.75643035625,57.0781249993855,-3.32347661575227));
#5354=CARTESIAN_POINT('Ctrl Pts',(-5.75643035625,57.1156249993855,-7.04959401029622E-16));
#5355=CARTESIAN_POINT('Ctrl Pts',(-5.75643035625,56.7781249993855,-7.04959401029622E-16));
#5356=CARTESIAN_POINT('Ctrl Pts',(-5.75643035625,56.8156249993855,3.32347661575227));
#5357=CARTESIAN_POINT('Ctrl Pts',(-2.878215178125,56.8531249993855,4.9852149236284));
#5358=CARTESIAN_POINT('Ctrl Pts',(-1.22102549985663E-15,56.8906249993855,
6.64695323150454));
#5359=CARTESIAN_POINT('Ctrl Pts',(2.878215178125,56.9281249993855,4.98521492362841));
#5360=CARTESIAN_POINT('Ctrl Pts',(5.75643035625,56.9656249993855,3.32347661575227));
#5361=CARTESIAN_POINT('Ctrl Pts',(5.75643035625,57.0031249993855,0.));
#5362=CARTESIAN_POINT('Ctrl Pts',(5.75643035625,57.0406249993855,-3.32347661575227));
#5363=CARTESIAN_POINT('Ctrl Pts',(2.878215178125,57.0781249993855,-4.9852149236284));
#5364=CARTESIAN_POINT('Ctrl Pts',(4.0700849995221E-16,57.1156249993855,
-6.64695323150454));
#5365=CARTESIAN_POINT('Ctrl Pts',(-2.878215178125,57.1531249993855,-4.9852149236284));
#5366=CARTESIAN_POINT('Ctrl Pts',(-5.75643035625,57.1906249993855,-3.32347661575227));
#5367=CARTESIAN_POINT('Ctrl Pts',(-5.75643035625,57.2281249993855,-7.04959401029622E-16));
#5368=CARTESIAN_POINT('Origin',(-2.22044604925031E-15,50.1968749993855,
-2.77555756156289E-16));
#5369=CARTESIAN_POINT('',(-5.75643035625,56.2156249993855,-9.82515157185911E-16));
#5370=CARTESIAN_POINT('',(-5.75643035625,56.3281249993855,-9.82515157185911E-16));
#5371=CARTESIAN_POINT('',(-5.75643035625,50.1968749993855,-1.2600709133422E-15));
#5372=CARTESIAN_POINT('Ctrl Pts',(-5.75643035625,56.2156249993855,-7.04959401029622E-16));
#5373=CARTESIAN_POINT('Ctrl Pts',(-5.75643035625,56.2531249993855,3.32347661575227));
#5374=CARTESIAN_POINT('Ctrl Pts',(-2.878215178125,56.2906249993855,4.9852149236284));
#5375=CARTESIAN_POINT('Ctrl Pts',(-1.22102549985663E-15,56.3281249993855,
6.64695323150454));
#5376=CARTESIAN_POINT('Ctrl Pts',(2.878215178125,56.3656249993855,4.98521492362841));
#5377=CARTESIAN_POINT('Ctrl Pts',(5.75643035625,56.4031249993855,3.32347661575227));
#5378=CARTESIAN_POINT('Ctrl Pts',(5.75643035625,56.4406249993855,0.));
#5379=CARTESIAN_POINT('Ctrl Pts',(5.75643035625,56.4781249993855,-3.32347661575227));
#5380=CARTESIAN_POINT('Ctrl Pts',(2.878215178125,56.5156249993855,-4.9852149236284));
#5381=CARTESIAN_POINT('Ctrl Pts',(4.0700849995221E-16,56.5531249993855,
-6.64695323150454));
#5382=CARTESIAN_POINT('Ctrl Pts',(-2.878215178125,56.5906249993855,-4.9852149236284));
#5383=CARTESIAN_POINT('Ctrl Pts',(-5.75643035625,56.6281249993855,-3.32347661575227));
#5384=CARTESIAN_POINT('Ctrl Pts',(-5.75643035625,56.6656249993855,-7.04959401029622E-16));
#5385=CARTESIAN_POINT('Ctrl Pts',(-5.75643035625,56.3281249993855,-7.04959401029622E-16));
#5386=CARTESIAN_POINT('Ctrl Pts',(-5.75643035625,56.3656249993855,3.32347661575227));
#5387=CARTESIAN_POINT('Ctrl Pts',(-2.878215178125,56.4031249993855,4.9852149236284));
#5388=CARTESIAN_POINT('Ctrl Pts',(-1.22102549985663E-15,56.4406249993855,
6.64695323150454));
#5389=CARTESIAN_POINT('Ctrl Pts',(2.878215178125,56.4781249993855,4.98521492362841));
#5390=CARTESIAN_POINT('Ctrl Pts',(5.75643035625,56.5156249993855,3.32347661575227));
#5391=CARTESIAN_POINT('Ctrl Pts',(5.75643035625,56.5531249993855,0.));
#5392=CARTESIAN_POINT('Ctrl Pts',(5.75643035625,56.5906249993855,-3.32347661575227));
#5393=CARTESIAN_POINT('Ctrl Pts',(2.878215178125,56.6281249993855,-4.9852149236284));
#5394=CARTESIAN_POINT('Ctrl Pts',(4.0700849995221E-16,56.6656249993855,
-6.64695323150454));
#5395=CARTESIAN_POINT('Ctrl Pts',(-2.878215178125,56.7031249993855,-4.9852149236284));
#5396=CARTESIAN_POINT('Ctrl Pts',(-5.75643035625,56.7406249993855,-3.32347661575227));
#5397=CARTESIAN_POINT('Ctrl Pts',(-5.75643035625,56.7781249993855,-7.04959401029622E-16));
#5398=CARTESIAN_POINT('Origin',(-2.22044604925031E-15,50.1968749993855,
-2.77555756156289E-16));
#5399=CARTESIAN_POINT('',(-5.75643035625,55.7656249993855,-9.82515157185911E-16));
#5400=CARTESIAN_POINT('',(-5.75643035625,55.8781249993855,-9.82515157185911E-16));
#5401=CARTESIAN_POINT('',(-5.75643035625,50.1968749993855,-1.2600709133422E-15));
#5402=CARTESIAN_POINT('Ctrl Pts',(-5.75643035625,55.7656249993855,-7.04959401029622E-16));
#5403=CARTESIAN_POINT('Ctrl Pts',(-5.75643035625,55.8031249993855,3.32347661575227));
#5404=CARTESIAN_POINT('Ctrl Pts',(-2.878215178125,55.8406249993855,4.9852149236284));
#5405=CARTESIAN_POINT('Ctrl Pts',(-1.22102549985663E-15,55.8781249993855,
6.64695323150454));
#5406=CARTESIAN_POINT('Ctrl Pts',(2.878215178125,55.9156249993855,4.98521492362841));
#5407=CARTESIAN_POINT('Ctrl Pts',(5.75643035625,55.9531249993855,3.32347661575227));
#5408=CARTESIAN_POINT('Ctrl Pts',(5.75643035625,55.9906249993855,0.));
#5409=CARTESIAN_POINT('Ctrl Pts',(5.75643035625,56.0281249993855,-3.32347661575227));
#5410=CARTESIAN_POINT('Ctrl Pts',(2.878215178125,56.0656249993855,-4.9852149236284));
#5411=CARTESIAN_POINT('Ctrl Pts',(4.0700849995221E-16,56.1031249993855,
-6.64695323150454));
#5412=CARTESIAN_POINT('Ctrl Pts',(-2.878215178125,56.1406249993855,-4.9852149236284));
#5413=CARTESIAN_POINT('Ctrl Pts',(-5.75643035625,56.1781249993855,-3.32347661575227));
#5414=CARTESIAN_POINT('Ctrl Pts',(-5.75643035625,56.2156249993855,-7.04959401029622E-16));
#5415=CARTESIAN_POINT('Ctrl Pts',(-5.75643035625,55.8781249993855,-7.04959401029622E-16));
#5416=CARTESIAN_POINT('Ctrl Pts',(-5.75643035625,55.9156249993855,3.32347661575227));
#5417=CARTESIAN_POINT('Ctrl Pts',(-2.878215178125,55.9531249993855,4.9852149236284));
#5418=CARTESIAN_POINT('Ctrl Pts',(-1.22102549985663E-15,55.9906249993855,
6.64695323150454));
#5419=CARTESIAN_POINT('Ctrl Pts',(2.878215178125,56.0281249993855,4.98521492362841));
#5420=CARTESIAN_POINT('Ctrl Pts',(5.75643035625,56.0656249993855,3.32347661575227));
#5421=CARTESIAN_POINT('Ctrl Pts',(5.75643035625,56.1031249993855,0.));
#5422=CARTESIAN_POINT('Ctrl Pts',(5.75643035625,56.1406249993855,-3.32347661575227));
#5423=CARTESIAN_POINT('Ctrl Pts',(2.878215178125,56.1781249993855,-4.9852149236284));
#5424=CARTESIAN_POINT('Ctrl Pts',(4.0700849995221E-16,56.2156249993855,
-6.64695323150454));
#5425=CARTESIAN_POINT('Ctrl Pts',(-2.878215178125,56.2531249993855,-4.9852149236284));
#5426=CARTESIAN_POINT('Ctrl Pts',(-5.75643035625,56.2906249993855,-3.32347661575227));
#5427=CARTESIAN_POINT('Ctrl Pts',(-5.75643035625,56.3281249993855,-7.04959401029622E-16));
#5428=CARTESIAN_POINT('Origin',(-2.22044604925031E-15,50.1968749993855,
-2.77555756156289E-16));
#5429=CARTESIAN_POINT('',(-5.75643035625,55.3156249993855,-9.82515157185911E-16));
#5430=CARTESIAN_POINT('',(-5.75643035625,55.4281249993855,-9.82515157185911E-16));
#5431=CARTESIAN_POINT('',(-5.75643035625,50.1968749993855,-1.2600709133422E-15));
#5432=CARTESIAN_POINT('Ctrl Pts',(-5.75643035625,55.3156249993855,-7.04959401029622E-16));
#5433=CARTESIAN_POINT('Ctrl Pts',(-5.75643035625,55.3531249993855,3.32347661575227));
#5434=CARTESIAN_POINT('Ctrl Pts',(-2.878215178125,55.3906249993855,4.9852149236284));
#5435=CARTESIAN_POINT('Ctrl Pts',(-1.22102549985663E-15,55.4281249993855,
6.64695323150454));
#5436=CARTESIAN_POINT('Ctrl Pts',(2.878215178125,55.4656249993855,4.98521492362841));
#5437=CARTESIAN_POINT('Ctrl Pts',(5.75643035625,55.5031249993855,3.32347661575227));
#5438=CARTESIAN_POINT('Ctrl Pts',(5.75643035625,55.5406249993855,0.));
#5439=CARTESIAN_POINT('Ctrl Pts',(5.75643035625,55.5781249993855,-3.32347661575227));
#5440=CARTESIAN_POINT('Ctrl Pts',(2.878215178125,55.6156249993855,-4.9852149236284));
#5441=CARTESIAN_POINT('Ctrl Pts',(4.0700849995221E-16,55.6531249993855,
-6.64695323150454));
#5442=CARTESIAN_POINT('Ctrl Pts',(-2.878215178125,55.6906249993855,-4.9852149236284));
#5443=CARTESIAN_POINT('Ctrl Pts',(-5.75643035625,55.7281249993855,-3.32347661575227));
#5444=CARTESIAN_POINT('Ctrl Pts',(-5.75643035625,55.7656249993855,-7.04959401029622E-16));
#5445=CARTESIAN_POINT('Ctrl Pts',(-5.75643035625,55.4281249993855,-7.04959401029622E-16));
#5446=CARTESIAN_POINT('Ctrl Pts',(-5.75643035625,55.4656249993855,3.32347661575227));
#5447=CARTESIAN_POINT('Ctrl Pts',(-2.878215178125,55.5031249993855,4.9852149236284));
#5448=CARTESIAN_POINT('Ctrl Pts',(-1.22102549985663E-15,55.5406249993855,
6.64695323150454));
#5449=CARTESIAN_POINT('Ctrl Pts',(2.878215178125,55.5781249993855,4.98521492362841));
#5450=CARTESIAN_POINT('Ctrl Pts',(5.75643035625,55.6156249993855,3.32347661575227));
#5451=CARTESIAN_POINT('Ctrl Pts',(5.75643035625,55.6531249993855,0.));
#5452=CARTESIAN_POINT('Ctrl Pts',(5.75643035625,55.6906249993855,-3.32347661575227));
#5453=CARTESIAN_POINT('Ctrl Pts',(2.878215178125,55.7281249993855,-4.9852149236284));
#5454=CARTESIAN_POINT('Ctrl Pts',(4.0700849995221E-16,55.7656249993855,
-6.64695323150454));
#5455=CARTESIAN_POINT('Ctrl Pts',(-2.878215178125,55.8031249993855,-4.9852149236284));
#5456=CARTESIAN_POINT('Ctrl Pts',(-5.75643035625,55.8406249993855,-3.32347661575227));
#5457=CARTESIAN_POINT('Ctrl Pts',(-5.75643035625,55.8781249993855,-7.04959401029622E-16));
#5458=CARTESIAN_POINT('Origin',(-2.22044604925031E-15,50.1968749993855,
-2.77555756156289E-16));
#5459=CARTESIAN_POINT('',(-5.75643035625,54.8656249993855,-9.82515157185911E-16));
#5460=CARTESIAN_POINT('',(-5.75643035625,54.9781249993855,-9.82515157185911E-16));
#5461=CARTESIAN_POINT('',(-5.75643035625,50.1968749993855,-1.2600709133422E-15));
#5462=CARTESIAN_POINT('Ctrl Pts',(-5.75643035625,54.8656249993855,-7.04959401029622E-16));
#5463=CARTESIAN_POINT('Ctrl Pts',(-5.75643035625,54.9031249993855,3.32347661575227));
#5464=CARTESIAN_POINT('Ctrl Pts',(-2.878215178125,54.9406249993855,4.9852149236284));
#5465=CARTESIAN_POINT('Ctrl Pts',(-1.22102549985663E-15,54.9781249993855,
6.64695323150454));
#5466=CARTESIAN_POINT('Ctrl Pts',(2.878215178125,55.0156249993855,4.98521492362841));
#5467=CARTESIAN_POINT('Ctrl Pts',(5.75643035625,55.0531249993855,3.32347661575227));
#5468=CARTESIAN_POINT('Ctrl Pts',(5.75643035625,55.0906249993855,0.));
#5469=CARTESIAN_POINT('Ctrl Pts',(5.75643035625,55.1281249993855,-3.32347661575227));
#5470=CARTESIAN_POINT('Ctrl Pts',(2.878215178125,55.1656249993855,-4.9852149236284));
#5471=CARTESIAN_POINT('Ctrl Pts',(4.0700849995221E-16,55.2031249993855,
-6.64695323150454));
#5472=CARTESIAN_POINT('Ctrl Pts',(-2.878215178125,55.2406249993855,-4.9852149236284));
#5473=CARTESIAN_POINT('Ctrl Pts',(-5.75643035625,55.2781249993855,-3.32347661575227));
#5474=CARTESIAN_POINT('Ctrl Pts',(-5.75643035625,55.3156249993855,-7.04959401029622E-16));
#5475=CARTESIAN_POINT('Ctrl Pts',(-5.75643035625,54.9781249993855,-7.04959401029622E-16));
#5476=CARTESIAN_POINT('Ctrl Pts',(-5.75643035625,55.0156249993855,3.32347661575227));
#5477=CARTESIAN_POINT('Ctrl Pts',(-2.878215178125,55.0531249993855,4.9852149236284));
#5478=CARTESIAN_POINT('Ctrl Pts',(-1.22102549985663E-15,55.0906249993855,
6.64695323150454));
#5479=CARTESIAN_POINT('Ctrl Pts',(2.878215178125,55.1281249993855,4.98521492362841));
#5480=CARTESIAN_POINT('Ctrl Pts',(5.75643035625,55.1656249993855,3.32347661575227));
#5481=CARTESIAN_POINT('Ctrl Pts',(5.75643035625,55.2031249993855,0.));
#5482=CARTESIAN_POINT('Ctrl Pts',(5.75643035625,55.2406249993855,-3.32347661575227));
#5483=CARTESIAN_POINT('Ctrl Pts',(2.878215178125,55.2781249993855,-4.9852149236284));
#5484=CARTESIAN_POINT('Ctrl Pts',(4.0700849995221E-16,55.3156249993855,
-6.64695323150454));
#5485=CARTESIAN_POINT('Ctrl Pts',(-2.878215178125,55.3531249993855,-4.9852149236284));
#5486=CARTESIAN_POINT('Ctrl Pts',(-5.75643035625,55.3906249993855,-3.32347661575227));
#5487=CARTESIAN_POINT('Ctrl Pts',(-5.75643035625,55.4281249993855,-7.04959401029622E-16));
#5488=CARTESIAN_POINT('Origin',(-2.22044604925031E-15,50.1968749993855,
-2.77555756156289E-16));
#5489=CARTESIAN_POINT('',(-5.75643035625,54.4156249993855,-9.82515157185911E-16));
#5490=CARTESIAN_POINT('',(-5.75643035625,54.5281249993855,-9.82515157185911E-16));
#5491=CARTESIAN_POINT('',(-5.75643035625,50.1968749993855,-1.2600709133422E-15));
#5492=CARTESIAN_POINT('Ctrl Pts',(-5.75643035625,54.4156249993855,-7.04959401029622E-16));
#5493=CARTESIAN_POINT('Ctrl Pts',(-5.75643035625,54.4531249993855,3.32347661575227));
#5494=CARTESIAN_POINT('Ctrl Pts',(-2.878215178125,54.4906249993855,4.9852149236284));
#5495=CARTESIAN_POINT('Ctrl Pts',(-1.22102549985663E-15,54.5281249993855,
6.64695323150454));
#5496=CARTESIAN_POINT('Ctrl Pts',(2.878215178125,54.5656249993855,4.98521492362841));
#5497=CARTESIAN_POINT('Ctrl Pts',(5.75643035625,54.6031249993855,3.32347661575227));
#5498=CARTESIAN_POINT('Ctrl Pts',(5.75643035625,54.6406249993855,0.));
#5499=CARTESIAN_POINT('Ctrl Pts',(5.75643035625,54.6781249993855,-3.32347661575227));
#5500=CARTESIAN_POINT('Ctrl Pts',(2.878215178125,54.7156249993855,-4.9852149236284));
#5501=CARTESIAN_POINT('Ctrl Pts',(4.0700849995221E-16,54.7531249993855,
-6.64695323150454));
#5502=CARTESIAN_POINT('Ctrl Pts',(-2.878215178125,54.7906249993855,-4.9852149236284));
#5503=CARTESIAN_POINT('Ctrl Pts',(-5.75643035625,54.8281249993855,-3.32347661575227));
#5504=CARTESIAN_POINT('Ctrl Pts',(-5.75643035625,54.8656249993855,-7.04959401029622E-16));
#5505=CARTESIAN_POINT('Ctrl Pts',(-5.75643035625,54.5281249993855,-7.04959401029622E-16));
#5506=CARTESIAN_POINT('Ctrl Pts',(-5.75643035625,54.5656249993855,3.32347661575227));
#5507=CARTESIAN_POINT('Ctrl Pts',(-2.878215178125,54.6031249993855,4.9852149236284));
#5508=CARTESIAN_POINT('Ctrl Pts',(-1.22102549985663E-15,54.6406249993855,
6.64695323150454));
#5509=CARTESIAN_POINT('Ctrl Pts',(2.878215178125,54.6781249993855,4.98521492362841));
#5510=CARTESIAN_POINT('Ctrl Pts',(5.75643035625,54.7156249993855,3.32347661575227));
#5511=CARTESIAN_POINT('Ctrl Pts',(5.75643035625,54.7531249993855,0.));
#5512=CARTESIAN_POINT('Ctrl Pts',(5.75643035625,54.7906249993855,-3.32347661575227));
#5513=CARTESIAN_POINT('Ctrl Pts',(2.878215178125,54.8281249993855,-4.9852149236284));
#5514=CARTESIAN_POINT('Ctrl Pts',(4.0700849995221E-16,54.8656249993855,
-6.64695323150454));
#5515=CARTESIAN_POINT('Ctrl Pts',(-2.878215178125,54.9031249993855,-4.9852149236284));
#5516=CARTESIAN_POINT('Ctrl Pts',(-5.75643035625,54.9406249993855,-3.32347661575227));
#5517=CARTESIAN_POINT('Ctrl Pts',(-5.75643035625,54.9781249993855,-7.04959401029622E-16));
#5518=CARTESIAN_POINT('Origin',(-2.22044604925031E-15,50.1968749993855,
-2.77555756156289E-16));
#5519=CARTESIAN_POINT('',(-5.75643035625,53.9656249993855,-9.82515157185911E-16));
#5520=CARTESIAN_POINT('',(-5.75643035625,54.0781249993855,-9.82515157185911E-16));
#5521=CARTESIAN_POINT('',(-5.75643035625,50.1968749993855,-1.2600709133422E-15));
#5522=CARTESIAN_POINT('Ctrl Pts',(-5.75643035625,53.9656249993855,-7.04959401029622E-16));
#5523=CARTESIAN_POINT('Ctrl Pts',(-5.75643035625,54.0031249993855,3.32347661575227));
#5524=CARTESIAN_POINT('Ctrl Pts',(-2.878215178125,54.0406249993855,4.9852149236284));
#5525=CARTESIAN_POINT('Ctrl Pts',(-1.22102549985663E-15,54.0781249993855,
6.64695323150454));
#5526=CARTESIAN_POINT('Ctrl Pts',(2.878215178125,54.1156249993855,4.98521492362841));
#5527=CARTESIAN_POINT('Ctrl Pts',(5.75643035625,54.1531249993855,3.32347661575227));
#5528=CARTESIAN_POINT('Ctrl Pts',(5.75643035625,54.1906249993855,0.));
#5529=CARTESIAN_POINT('Ctrl Pts',(5.75643035625,54.2281249993855,-3.32347661575227));
#5530=CARTESIAN_POINT('Ctrl Pts',(2.878215178125,54.2656249993855,-4.9852149236284));
#5531=CARTESIAN_POINT('Ctrl Pts',(4.0700849995221E-16,54.3031249993855,
-6.64695323150454));
#5532=CARTESIAN_POINT('Ctrl Pts',(-2.878215178125,54.3406249993855,-4.9852149236284));
#5533=CARTESIAN_POINT('Ctrl Pts',(-5.75643035625,54.3781249993855,-3.32347661575227));
#5534=CARTESIAN_POINT('Ctrl Pts',(-5.75643035625,54.4156249993855,-7.04959401029622E-16));
#5535=CARTESIAN_POINT('Ctrl Pts',(-5.75643035625,54.0781249993855,-7.04959401029622E-16));
#5536=CARTESIAN_POINT('Ctrl Pts',(-5.75643035625,54.1156249993855,3.32347661575227));
#5537=CARTESIAN_POINT('Ctrl Pts',(-2.878215178125,54.1531249993855,4.9852149236284));
#5538=CARTESIAN_POINT('Ctrl Pts',(-1.22102549985663E-15,54.1906249993855,
6.64695323150454));
#5539=CARTESIAN_POINT('Ctrl Pts',(2.878215178125,54.2281249993855,4.98521492362841));
#5540=CARTESIAN_POINT('Ctrl Pts',(5.75643035625,54.2656249993855,3.32347661575227));
#5541=CARTESIAN_POINT('Ctrl Pts',(5.75643035625,54.3031249993855,0.));
#5542=CARTESIAN_POINT('Ctrl Pts',(5.75643035625,54.3406249993855,-3.32347661575227));
#5543=CARTESIAN_POINT('Ctrl Pts',(2.878215178125,54.3781249993855,-4.9852149236284));
#5544=CARTESIAN_POINT('Ctrl Pts',(4.0700849995221E-16,54.4156249993855,
-6.64695323150454));
#5545=CARTESIAN_POINT('Ctrl Pts',(-2.878215178125,54.4531249993855,-4.9852149236284));
#5546=CARTESIAN_POINT('Ctrl Pts',(-5.75643035625,54.4906249993855,-3.32347661575227));
#5547=CARTESIAN_POINT('Ctrl Pts',(-5.75643035625,54.5281249993855,-7.04959401029622E-16));
#5548=CARTESIAN_POINT('Origin',(-2.22044604925031E-15,50.1968749993855,
-2.77555756156289E-16));
#5549=CARTESIAN_POINT('',(-5.75643035625,53.5156249993855,-9.82515157185911E-16));
#5550=CARTESIAN_POINT('',(-5.75643035625,53.6281249993855,-9.82515157185911E-16));
#5551=CARTESIAN_POINT('',(-5.75643035625,50.1968749993855,-1.2600709133422E-15));
#5552=CARTESIAN_POINT('Ctrl Pts',(-5.75643035625,53.5156249993855,-7.04959401029622E-16));
#5553=CARTESIAN_POINT('Ctrl Pts',(-5.75643035625,53.5531249993855,3.32347661575227));
#5554=CARTESIAN_POINT('Ctrl Pts',(-2.878215178125,53.5906249993855,4.9852149236284));
#5555=CARTESIAN_POINT('Ctrl Pts',(-1.22102549985663E-15,53.6281249993855,
6.64695323150454));
#5556=CARTESIAN_POINT('Ctrl Pts',(2.878215178125,53.6656249993855,4.98521492362841));
#5557=CARTESIAN_POINT('Ctrl Pts',(5.75643035625,53.7031249993855,3.32347661575227));
#5558=CARTESIAN_POINT('Ctrl Pts',(5.75643035625,53.7406249993855,0.));
#5559=CARTESIAN_POINT('Ctrl Pts',(5.75643035625,53.7781249993855,-3.32347661575227));
#5560=CARTESIAN_POINT('Ctrl Pts',(2.878215178125,53.8156249993855,-4.9852149236284));
#5561=CARTESIAN_POINT('Ctrl Pts',(4.0700849995221E-16,53.8531249993855,
-6.64695323150454));
#5562=CARTESIAN_POINT('Ctrl Pts',(-2.878215178125,53.8906249993855,-4.9852149236284));
#5563=CARTESIAN_POINT('Ctrl Pts',(-5.75643035625,53.9281249993855,-3.32347661575227));
#5564=CARTESIAN_POINT('Ctrl Pts',(-5.75643035625,53.9656249993855,-7.04959401029622E-16));
#5565=CARTESIAN_POINT('Ctrl Pts',(-5.75643035625,53.6281249993855,-7.04959401029622E-16));
#5566=CARTESIAN_POINT('Ctrl Pts',(-5.75643035625,53.6656249993855,3.32347661575227));
#5567=CARTESIAN_POINT('Ctrl Pts',(-2.878215178125,53.7031249993855,4.9852149236284));
#5568=CARTESIAN_POINT('Ctrl Pts',(-1.22102549985663E-15,53.7406249993855,
6.64695323150454));
#5569=CARTESIAN_POINT('Ctrl Pts',(2.878215178125,53.7781249993855,4.98521492362841));
#5570=CARTESIAN_POINT('Ctrl Pts',(5.75643035625,53.8156249993855,3.32347661575227));
#5571=CARTESIAN_POINT('Ctrl Pts',(5.75643035625,53.8531249993855,0.));
#5572=CARTESIAN_POINT('Ctrl Pts',(5.75643035625,53.8906249993855,-3.32347661575227));
#5573=CARTESIAN_POINT('Ctrl Pts',(2.878215178125,53.9281249993855,-4.9852149236284));
#5574=CARTESIAN_POINT('Ctrl Pts',(4.0700849995221E-16,53.9656249993855,
-6.64695323150454));
#5575=CARTESIAN_POINT('Ctrl Pts',(-2.878215178125,54.0031249993855,-4.9852149236284));
#5576=CARTESIAN_POINT('Ctrl Pts',(-5.75643035625,54.0406249993855,-3.32347661575227));
#5577=CARTESIAN_POINT('Ctrl Pts',(-5.75643035625,54.0781249993855,-7.04959401029622E-16));
#5578=CARTESIAN_POINT('Origin',(-2.22044604925031E-15,50.1968749993855,
-2.77555756156289E-16));
#5579=CARTESIAN_POINT('',(-5.75643035625,53.0656249993855,-9.82515157185911E-16));
#5580=CARTESIAN_POINT('',(-5.75643035625,53.1781249993855,-9.82515157185911E-16));
#5581=CARTESIAN_POINT('',(-5.75643035625,50.1968749993855,-1.2600709133422E-15));
#5582=CARTESIAN_POINT('Ctrl Pts',(-5.75643035625,53.0656249993855,-7.04959401029622E-16));
#5583=CARTESIAN_POINT('Ctrl Pts',(-5.75643035625,53.1031249993855,3.32347661575227));
#5584=CARTESIAN_POINT('Ctrl Pts',(-2.878215178125,53.1406249993855,4.9852149236284));
#5585=CARTESIAN_POINT('Ctrl Pts',(-1.22102549985663E-15,53.1781249993855,
6.64695323150454));
#5586=CARTESIAN_POINT('Ctrl Pts',(2.878215178125,53.2156249993855,4.98521492362841));
#5587=CARTESIAN_POINT('Ctrl Pts',(5.75643035625,53.2531249993855,3.32347661575227));
#5588=CARTESIAN_POINT('Ctrl Pts',(5.75643035625,53.2906249993855,0.));
#5589=CARTESIAN_POINT('Ctrl Pts',(5.75643035625,53.3281249993855,-3.32347661575227));
#5590=CARTESIAN_POINT('Ctrl Pts',(2.878215178125,53.3656249993855,-4.9852149236284));
#5591=CARTESIAN_POINT('Ctrl Pts',(4.0700849995221E-16,53.4031249993855,
-6.64695323150454));
#5592=CARTESIAN_POINT('Ctrl Pts',(-2.878215178125,53.4406249993855,-4.9852149236284));
#5593=CARTESIAN_POINT('Ctrl Pts',(-5.75643035625,53.4781249993855,-3.32347661575227));
#5594=CARTESIAN_POINT('Ctrl Pts',(-5.75643035625,53.5156249993855,-7.04959401029622E-16));
#5595=CARTESIAN_POINT('Ctrl Pts',(-5.75643035625,53.1781249993855,-7.04959401029622E-16));
#5596=CARTESIAN_POINT('Ctrl Pts',(-5.75643035625,53.2156249993855,3.32347661575227));
#5597=CARTESIAN_POINT('Ctrl Pts',(-2.878215178125,53.2531249993855,4.9852149236284));
#5598=CARTESIAN_POINT('Ctrl Pts',(-1.22102549985663E-15,53.2906249993855,
6.64695323150454));
#5599=CARTESIAN_POINT('Ctrl Pts',(2.878215178125,53.3281249993855,4.98521492362841));
#5600=CARTESIAN_POINT('Ctrl Pts',(5.75643035625,53.3656249993855,3.32347661575227));
#5601=CARTESIAN_POINT('Ctrl Pts',(5.75643035625,53.4031249993855,0.));
#5602=CARTESIAN_POINT('Ctrl Pts',(5.75643035625,53.4406249993855,-3.32347661575227));
#5603=CARTESIAN_POINT('Ctrl Pts',(2.878215178125,53.4781249993855,-4.9852149236284));
#5604=CARTESIAN_POINT('Ctrl Pts',(4.0700849995221E-16,53.5156249993855,
-6.64695323150454));
#5605=CARTESIAN_POINT('Ctrl Pts',(-2.878215178125,53.5531249993855,-4.9852149236284));
#5606=CARTESIAN_POINT('Ctrl Pts',(-5.75643035625,53.5906249993855,-3.32347661575227));
#5607=CARTESIAN_POINT('Ctrl Pts',(-5.75643035625,53.6281249993855,-7.04959401029622E-16));
#5608=CARTESIAN_POINT('Origin',(-2.22044604925031E-15,50.1968749993855,
-2.77555756156289E-16));
#5609=CARTESIAN_POINT('',(-5.75643035625,52.6156249993855,-9.82515157185911E-16));
#5610=CARTESIAN_POINT('',(-5.75643035625,52.7281249993855,-9.82515157185911E-16));
#5611=CARTESIAN_POINT('',(-5.75643035625,50.1968749993855,-1.2600709133422E-15));
#5612=CARTESIAN_POINT('Ctrl Pts',(-5.75643035625,52.6156249993855,-7.04959401029622E-16));
#5613=CARTESIAN_POINT('Ctrl Pts',(-5.75643035625,52.6531249993855,3.32347661575227));
#5614=CARTESIAN_POINT('Ctrl Pts',(-2.878215178125,52.6906249993855,4.9852149236284));
#5615=CARTESIAN_POINT('Ctrl Pts',(-1.22102549985663E-15,52.7281249993855,
6.64695323150454));
#5616=CARTESIAN_POINT('Ctrl Pts',(2.878215178125,52.7656249993855,4.98521492362841));
#5617=CARTESIAN_POINT('Ctrl Pts',(5.75643035625,52.8031249993855,3.32347661575227));
#5618=CARTESIAN_POINT('Ctrl Pts',(5.75643035625,52.8406249993855,0.));
#5619=CARTESIAN_POINT('Ctrl Pts',(5.75643035625,52.8781249993855,-3.32347661575227));
#5620=CARTESIAN_POINT('Ctrl Pts',(2.878215178125,52.9156249993855,-4.9852149236284));
#5621=CARTESIAN_POINT('Ctrl Pts',(4.0700849995221E-16,52.9531249993855,
-6.64695323150454));
#5622=CARTESIAN_POINT('Ctrl Pts',(-2.878215178125,52.9906249993855,-4.9852149236284));
#5623=CARTESIAN_POINT('Ctrl Pts',(-5.75643035625,53.0281249993855,-3.32347661575227));
#5624=CARTESIAN_POINT('Ctrl Pts',(-5.75643035625,53.0656249993855,-7.04959401029622E-16));
#5625=CARTESIAN_POINT('Ctrl Pts',(-5.75643035625,52.7281249993855,-7.04959401029622E-16));
#5626=CARTESIAN_POINT('Ctrl Pts',(-5.75643035625,52.7656249993855,3.32347661575227));
#5627=CARTESIAN_POINT('Ctrl Pts',(-2.878215178125,52.8031249993855,4.9852149236284));
#5628=CARTESIAN_POINT('Ctrl Pts',(-1.22102549985663E-15,52.8406249993855,
6.64695323150454));
#5629=CARTESIAN_POINT('Ctrl Pts',(2.878215178125,52.8781249993855,4.98521492362841));
#5630=CARTESIAN_POINT('Ctrl Pts',(5.75643035625,52.9156249993855,3.32347661575227));
#5631=CARTESIAN_POINT('Ctrl Pts',(5.75643035625,52.9531249993855,0.));
#5632=CARTESIAN_POINT('Ctrl Pts',(5.75643035625,52.9906249993855,-3.32347661575227));
#5633=CARTESIAN_POINT('Ctrl Pts',(2.878215178125,53.0281249993855,-4.9852149236284));
#5634=CARTESIAN_POINT('Ctrl Pts',(4.0700849995221E-16,53.0656249993855,
-6.64695323150454));
#5635=CARTESIAN_POINT('Ctrl Pts',(-2.878215178125,53.1031249993855,-4.9852149236284));
#5636=CARTESIAN_POINT('Ctrl Pts',(-5.75643035625,53.1406249993855,-3.32347661575227));
#5637=CARTESIAN_POINT('Ctrl Pts',(-5.75643035625,53.1781249993855,-7.04959401029622E-16));
#5638=CARTESIAN_POINT('Origin',(-2.22044604925031E-15,50.1968749993855,
-2.77555756156289E-16));
#5639=CARTESIAN_POINT('',(-5.75643035625,52.1656249993855,-9.82515157185911E-16));
#5640=CARTESIAN_POINT('',(-5.75643035625,52.2781249993855,-9.82515157185911E-16));
#5641=CARTESIAN_POINT('',(-5.75643035625,50.1968749993855,-1.2600709133422E-15));
#5642=CARTESIAN_POINT('Ctrl Pts',(-5.75643035625,52.1656249993855,-7.04959401029622E-16));
#5643=CARTESIAN_POINT('Ctrl Pts',(-5.75643035625,52.2031249993855,3.32347661575227));
#5644=CARTESIAN_POINT('Ctrl Pts',(-2.878215178125,52.2406249993855,4.9852149236284));
#5645=CARTESIAN_POINT('Ctrl Pts',(-1.22102549985663E-15,52.2781249993855,
6.64695323150454));
#5646=CARTESIAN_POINT('Ctrl Pts',(2.878215178125,52.3156249993855,4.98521492362841));
#5647=CARTESIAN_POINT('Ctrl Pts',(5.75643035625,52.3531249993855,3.32347661575227));
#5648=CARTESIAN_POINT('Ctrl Pts',(5.75643035625,52.3906249993855,0.));
#5649=CARTESIAN_POINT('Ctrl Pts',(5.75643035625,52.4281249993855,-3.32347661575227));
#5650=CARTESIAN_POINT('Ctrl Pts',(2.878215178125,52.4656249993855,-4.9852149236284));
#5651=CARTESIAN_POINT('Ctrl Pts',(4.0700849995221E-16,52.5031249993855,
-6.64695323150454));
#5652=CARTESIAN_POINT('Ctrl Pts',(-2.878215178125,52.5406249993855,-4.9852149236284));
#5653=CARTESIAN_POINT('Ctrl Pts',(-5.75643035625,52.5781249993855,-3.32347661575227));
#5654=CARTESIAN_POINT('Ctrl Pts',(-5.75643035625,52.6156249993855,-7.04959401029622E-16));
#5655=CARTESIAN_POINT('Ctrl Pts',(-5.75643035625,52.2781249993855,-7.04959401029622E-16));
#5656=CARTESIAN_POINT('Ctrl Pts',(-5.75643035625,52.3156249993855,3.32347661575227));
#5657=CARTESIAN_POINT('Ctrl Pts',(-2.878215178125,52.3531249993855,4.9852149236284));
#5658=CARTESIAN_POINT('Ctrl Pts',(-1.22102549985663E-15,52.3906249993855,
6.64695323150454));
#5659=CARTESIAN_POINT('Ctrl Pts',(2.878215178125,52.4281249993855,4.98521492362841));
#5660=CARTESIAN_POINT('Ctrl Pts',(5.75643035625,52.4656249993855,3.32347661575227));
#5661=CARTESIAN_POINT('Ctrl Pts',(5.75643035625,52.5031249993855,0.));
#5662=CARTESIAN_POINT('Ctrl Pts',(5.75643035625,52.5406249993855,-3.32347661575227));
#5663=CARTESIAN_POINT('Ctrl Pts',(2.878215178125,52.5781249993855,-4.9852149236284));
#5664=CARTESIAN_POINT('Ctrl Pts',(4.0700849995221E-16,52.6156249993855,
-6.64695323150454));
#5665=CARTESIAN_POINT('Ctrl Pts',(-2.878215178125,52.6531249993855,-4.9852149236284));
#5666=CARTESIAN_POINT('Ctrl Pts',(-5.75643035625,52.6906249993855,-3.32347661575227));
#5667=CARTESIAN_POINT('Ctrl Pts',(-5.75643035625,52.7281249993855,-7.04959401029622E-16));
#5668=CARTESIAN_POINT('Origin',(-2.22044604925031E-15,50.1968749993855,
-2.77555756156289E-16));
#5669=CARTESIAN_POINT('',(-5.75643035625,51.7156249993855,-9.82515157185911E-16));
#5670=CARTESIAN_POINT('',(-5.75643035625,51.8281249993855,-9.82515157185911E-16));
#5671=CARTESIAN_POINT('',(-5.75643035625,50.1968749993855,-1.2600709133422E-15));
#5672=CARTESIAN_POINT('Ctrl Pts',(-5.75643035625,51.7156249993855,-7.04959401029622E-16));
#5673=CARTESIAN_POINT('Ctrl Pts',(-5.75643035625,51.7531249993855,3.32347661575227));
#5674=CARTESIAN_POINT('Ctrl Pts',(-2.878215178125,51.7906249993855,4.9852149236284));
#5675=CARTESIAN_POINT('Ctrl Pts',(-1.22102549985663E-15,51.8281249993855,
6.64695323150454));
#5676=CARTESIAN_POINT('Ctrl Pts',(2.878215178125,51.8656249993855,4.98521492362841));
#5677=CARTESIAN_POINT('Ctrl Pts',(5.75643035625,51.9031249993855,3.32347661575227));
#5678=CARTESIAN_POINT('Ctrl Pts',(5.75643035625,51.9406249993855,0.));
#5679=CARTESIAN_POINT('Ctrl Pts',(5.75643035625,51.9781249993855,-3.32347661575227));
#5680=CARTESIAN_POINT('Ctrl Pts',(2.878215178125,52.0156249993855,-4.9852149236284));
#5681=CARTESIAN_POINT('Ctrl Pts',(4.0700849995221E-16,52.0531249993855,
-6.64695323150454));
#5682=CARTESIAN_POINT('Ctrl Pts',(-2.878215178125,52.0906249993855,-4.9852149236284));
#5683=CARTESIAN_POINT('Ctrl Pts',(-5.75643035625,52.1281249993855,-3.32347661575227));
#5684=CARTESIAN_POINT('Ctrl Pts',(-5.75643035625,52.1656249993855,-7.04959401029622E-16));
#5685=CARTESIAN_POINT('Ctrl Pts',(-5.75643035625,51.8281249993855,-7.04959401029622E-16));
#5686=CARTESIAN_POINT('Ctrl Pts',(-5.75643035625,51.8656249993855,3.32347661575227));
#5687=CARTESIAN_POINT('Ctrl Pts',(-2.878215178125,51.9031249993855,4.9852149236284));
#5688=CARTESIAN_POINT('Ctrl Pts',(-1.22102549985663E-15,51.9406249993855,
6.64695323150454));
#5689=CARTESIAN_POINT('Ctrl Pts',(2.878215178125,51.9781249993855,4.98521492362841));
#5690=CARTESIAN_POINT('Ctrl Pts',(5.75643035625,52.0156249993855,3.32347661575227));
#5691=CARTESIAN_POINT('Ctrl Pts',(5.75643035625,52.0531249993855,0.));
#5692=CARTESIAN_POINT('Ctrl Pts',(5.75643035625,52.0906249993855,-3.32347661575227));
#5693=CARTESIAN_POINT('Ctrl Pts',(2.878215178125,52.1281249993855,-4.9852149236284));
#5694=CARTESIAN_POINT('Ctrl Pts',(4.0700849995221E-16,52.1656249993855,
-6.64695323150454));
#5695=CARTESIAN_POINT('Ctrl Pts',(-2.878215178125,52.2031249993855,-4.9852149236284));
#5696=CARTESIAN_POINT('Ctrl Pts',(-5.75643035625,52.2406249993855,-3.32347661575227));
#5697=CARTESIAN_POINT('Ctrl Pts',(-5.75643035625,52.2781249993855,-7.04959401029622E-16));
#5698=CARTESIAN_POINT('Origin',(-2.22044604925031E-15,50.1968749993855,
-2.77555756156289E-16));
#5699=CARTESIAN_POINT('',(-5.75643035625,51.2656249993855,-9.82515157185911E-16));
#5700=CARTESIAN_POINT('',(-5.75643035625,51.3781249993855,-9.82515157185911E-16));
#5701=CARTESIAN_POINT('',(-5.75643035625,50.1968749993855,-1.2600709133422E-15));
#5702=CARTESIAN_POINT('Ctrl Pts',(-5.75643035625,51.2656249993855,-7.04959401029622E-16));
#5703=CARTESIAN_POINT('Ctrl Pts',(-5.75643035625,51.3031249993855,3.32347661575227));
#5704=CARTESIAN_POINT('Ctrl Pts',(-2.878215178125,51.3406249993855,4.9852149236284));
#5705=CARTESIAN_POINT('Ctrl Pts',(-1.22102549985663E-15,51.3781249993855,
6.64695323150454));
#5706=CARTESIAN_POINT('Ctrl Pts',(2.878215178125,51.4156249993855,4.98521492362841));
#5707=CARTESIAN_POINT('Ctrl Pts',(5.75643035625,51.4531249993855,3.32347661575227));
#5708=CARTESIAN_POINT('Ctrl Pts',(5.75643035625,51.4906249993855,0.));
#5709=CARTESIAN_POINT('Ctrl Pts',(5.75643035625,51.5281249993855,-3.32347661575227));
#5710=CARTESIAN_POINT('Ctrl Pts',(2.878215178125,51.5656249993855,-4.9852149236284));
#5711=CARTESIAN_POINT('Ctrl Pts',(4.0700849995221E-16,51.6031249993855,
-6.64695323150454));
#5712=CARTESIAN_POINT('Ctrl Pts',(-2.878215178125,51.6406249993855,-4.9852149236284));
#5713=CARTESIAN_POINT('Ctrl Pts',(-5.75643035625,51.6781249993855,-3.32347661575227));
#5714=CARTESIAN_POINT('Ctrl Pts',(-5.75643035625,51.7156249993855,-7.04959401029622E-16));
#5715=CARTESIAN_POINT('Ctrl Pts',(-5.75643035625,51.3781249993855,-7.04959401029622E-16));
#5716=CARTESIAN_POINT('Ctrl Pts',(-5.75643035625,51.4156249993855,3.32347661575227));
#5717=CARTESIAN_POINT('Ctrl Pts',(-2.878215178125,51.4531249993855,4.9852149236284));
#5718=CARTESIAN_POINT('Ctrl Pts',(-1.22102549985663E-15,51.4906249993855,
6.64695323150454));
#5719=CARTESIAN_POINT('Ctrl Pts',(2.878215178125,51.5281249993855,4.98521492362841));
#5720=CARTESIAN_POINT('Ctrl Pts',(5.75643035625,51.5656249993855,3.32347661575227));
#5721=CARTESIAN_POINT('Ctrl Pts',(5.75643035625,51.6031249993855,0.));
#5722=CARTESIAN_POINT('Ctrl Pts',(5.75643035625,51.6406249993855,-3.32347661575227));
#5723=CARTESIAN_POINT('Ctrl Pts',(2.878215178125,51.6781249993855,-4.9852149236284));
#5724=CARTESIAN_POINT('Ctrl Pts',(4.0700849995221E-16,51.7156249993855,
-6.64695323150454));
#5725=CARTESIAN_POINT('Ctrl Pts',(-2.878215178125,51.7531249993855,-4.9852149236284));
#5726=CARTESIAN_POINT('Ctrl Pts',(-5.75643035625,51.7906249993855,-3.32347661575227));
#5727=CARTESIAN_POINT('Ctrl Pts',(-5.75643035625,51.8281249993855,-7.04959401029622E-16));
#5728=CARTESIAN_POINT('Origin',(-2.22044604925031E-15,50.1968749993855,
-2.77555756156289E-16));
#5729=CARTESIAN_POINT('',(-5.75643035625,50.8156249993855,-9.82515157185911E-16));
#5730=CARTESIAN_POINT('',(-5.75643035625,50.9281249993855,-9.82515157185911E-16));
#5731=CARTESIAN_POINT('',(-5.75643035625,50.1968749993855,-1.2600709133422E-15));
#5732=CARTESIAN_POINT('Ctrl Pts',(-5.75643035625,50.8156249993855,-7.04959401029622E-16));
#5733=CARTESIAN_POINT('Ctrl Pts',(-5.75643035625,50.8531249993855,3.32347661575227));
#5734=CARTESIAN_POINT('Ctrl Pts',(-2.878215178125,50.8906249993855,4.9852149236284));
#5735=CARTESIAN_POINT('Ctrl Pts',(-1.22102549985663E-15,50.9281249993855,
6.64695323150454));
#5736=CARTESIAN_POINT('Ctrl Pts',(2.878215178125,50.9656249993855,4.98521492362841));
#5737=CARTESIAN_POINT('Ctrl Pts',(5.75643035625,51.0031249993855,3.32347661575227));
#5738=CARTESIAN_POINT('Ctrl Pts',(5.75643035625,51.0406249993855,0.));
#5739=CARTESIAN_POINT('Ctrl Pts',(5.75643035625,51.0781249993855,-3.32347661575227));
#5740=CARTESIAN_POINT('Ctrl Pts',(2.878215178125,51.1156249993855,-4.9852149236284));
#5741=CARTESIAN_POINT('Ctrl Pts',(4.0700849995221E-16,51.1531249993855,
-6.64695323150454));
#5742=CARTESIAN_POINT('Ctrl Pts',(-2.878215178125,51.1906249993855,-4.9852149236284));
#5743=CARTESIAN_POINT('Ctrl Pts',(-5.75643035625,51.2281249993855,-3.32347661575227));
#5744=CARTESIAN_POINT('Ctrl Pts',(-5.75643035625,51.2656249993855,-7.04959401029622E-16));
#5745=CARTESIAN_POINT('Ctrl Pts',(-5.75643035625,50.9281249993855,-7.04959401029622E-16));
#5746=CARTESIAN_POINT('Ctrl Pts',(-5.75643035625,50.9656249993855,3.32347661575227));
#5747=CARTESIAN_POINT('Ctrl Pts',(-2.878215178125,51.0031249993855,4.9852149236284));
#5748=CARTESIAN_POINT('Ctrl Pts',(-1.22102549985663E-15,51.0406249993855,
6.64695323150454));
#5749=CARTESIAN_POINT('Ctrl Pts',(2.878215178125,51.0781249993855,4.98521492362841));
#5750=CARTESIAN_POINT('Ctrl Pts',(5.75643035625,51.1156249993855,3.32347661575227));
#5751=CARTESIAN_POINT('Ctrl Pts',(5.75643035625,51.1531249993855,0.));
#5752=CARTESIAN_POINT('Ctrl Pts',(5.75643035625,51.1906249993855,-3.32347661575227));
#5753=CARTESIAN_POINT('Ctrl Pts',(2.878215178125,51.2281249993855,-4.9852149236284));
#5754=CARTESIAN_POINT('Ctrl Pts',(4.0700849995221E-16,51.2656249993855,
-6.64695323150454));
#5755=CARTESIAN_POINT('Ctrl Pts',(-2.878215178125,51.3031249993855,-4.9852149236284));
#5756=CARTESIAN_POINT('Ctrl Pts',(-5.75643035625,51.3406249993855,-3.32347661575227));
#5757=CARTESIAN_POINT('Ctrl Pts',(-5.75643035625,51.3781249993855,-7.04959401029622E-16));
#5758=CARTESIAN_POINT('Origin',(-2.22044604925031E-15,50.1968749993855,
-2.77555756156289E-16));
#5759=CARTESIAN_POINT('',(-5.75643035625,50.3656249993855,-9.82515157185911E-16));
#5760=CARTESIAN_POINT('',(-5.75643035625,50.4781249993855,-9.82515157185911E-16));
#5761=CARTESIAN_POINT('',(-5.75643035625,50.1968749993855,-1.2600709133422E-15));
#5762=CARTESIAN_POINT('Ctrl Pts',(-5.75643035625,50.3656249993855,-7.04959401029622E-16));
#5763=CARTESIAN_POINT('Ctrl Pts',(-5.75643035625,50.4031249993855,3.32347661575227));
#5764=CARTESIAN_POINT('Ctrl Pts',(-2.878215178125,50.4406249993855,4.9852149236284));
#5765=CARTESIAN_POINT('Ctrl Pts',(-1.22102549985663E-15,50.4781249993855,
6.64695323150454));
#5766=CARTESIAN_POINT('Ctrl Pts',(2.878215178125,50.5156249993855,4.98521492362841));
#5767=CARTESIAN_POINT('Ctrl Pts',(5.75643035625,50.5531249993855,3.32347661575227));
#5768=CARTESIAN_POINT('Ctrl Pts',(5.75643035625,50.5906249993855,0.));
#5769=CARTESIAN_POINT('Ctrl Pts',(5.75643035625,50.6281249993855,-3.32347661575227));
#5770=CARTESIAN_POINT('Ctrl Pts',(2.878215178125,50.6656249993855,-4.9852149236284));
#5771=CARTESIAN_POINT('Ctrl Pts',(4.0700849995221E-16,50.7031249993855,
-6.64695323150454));
#5772=CARTESIAN_POINT('Ctrl Pts',(-2.878215178125,50.7406249993855,-4.9852149236284));
#5773=CARTESIAN_POINT('Ctrl Pts',(-5.75643035625,50.7781249993855,-3.32347661575227));
#5774=CARTESIAN_POINT('Ctrl Pts',(-5.75643035625,50.8156249993855,-7.04959401029622E-16));
#5775=CARTESIAN_POINT('Ctrl Pts',(-5.75643035625,50.4781249993855,-7.04959401029622E-16));
#5776=CARTESIAN_POINT('Ctrl Pts',(-5.75643035625,50.5156249993855,3.32347661575227));
#5777=CARTESIAN_POINT('Ctrl Pts',(-2.878215178125,50.5531249993855,4.9852149236284));
#5778=CARTESIAN_POINT('Ctrl Pts',(-1.22102549985663E-15,50.5906249993855,
6.64695323150454));
#5779=CARTESIAN_POINT('Ctrl Pts',(2.878215178125,50.6281249993855,4.98521492362841));
#5780=CARTESIAN_POINT('Ctrl Pts',(5.75643035625,50.6656249993855,3.32347661575227));
#5781=CARTESIAN_POINT('Ctrl Pts',(5.75643035625,50.7031249993855,0.));
#5782=CARTESIAN_POINT('Ctrl Pts',(5.75643035625,50.7406249993855,-3.32347661575227));
#5783=CARTESIAN_POINT('Ctrl Pts',(2.878215178125,50.7781249993855,-4.9852149236284));
#5784=CARTESIAN_POINT('Ctrl Pts',(4.0700849995221E-16,50.8156249993855,
-6.64695323150454));
#5785=CARTESIAN_POINT('Ctrl Pts',(-2.878215178125,50.8531249993855,-4.9852149236284));
#5786=CARTESIAN_POINT('Ctrl Pts',(-5.75643035625,50.8906249993855,-3.32347661575227));
#5787=CARTESIAN_POINT('Ctrl Pts',(-5.75643035625,50.9281249993855,-7.04959401029622E-16));
#5788=CARTESIAN_POINT('Origin',(0.,50.,0.));
#5789=CARTESIAN_POINT('',(-1.07185518347685E-16,50.1125,-6.));
#5790=CARTESIAN_POINT('',(-7.34788079488412E-16,50.,-6.));
#5791=CARTESIAN_POINT('',(-7.34788079488412E-16,50.,-6.));
#5792=CARTESIAN_POINT('',(6.,50.,0.));
#5793=CARTESIAN_POINT('Ctrl Pts',(7.63278329429795E-16,50.1125,-6.));
#5794=CARTESIAN_POINT('Ctrl Pts',(0.343291227172437,50.1082088596603,-6.));
#5795=CARTESIAN_POINT('Ctrl Pts',(0.686759034749955,50.1039155120655,-5.97053821667675));
#5796=CARTESIAN_POINT('Ctrl Pts',(1.77491233708495,50.0903135957864,-5.78157134708829));
#5797=CARTESIAN_POINT('Ctrl Pts',(2.49179065334938,50.0815813989611,-5.51070121351748));
#5798=CARTESIAN_POINT('Ctrl Pts',(3.81594411981456,50.0645056281562,-4.69780943448951));
#5799=CARTESIAN_POINT('Ctrl Pts',(4.40362359624846,50.0549238334303,-4.15197805611787));
#5800=CARTESIAN_POINT('Ctrl Pts',(5.23987317830986,50.0371337154915,-2.99140627649053));
#5801=CARTESIAN_POINT('Ctrl Pts',(5.52735144341947,50.0291440981232,-2.41933269210065));
#5802=CARTESIAN_POINT('Ctrl Pts',(5.905418894506,50.0138685530285,-1.2265156251652));
#5803=CARTESIAN_POINT('Ctrl Pts',(6.,50.0066584470657,-0.615080992922631));
#5804=CARTESIAN_POINT('Ctrl Pts',(6.,50.,0.));
#5805=CARTESIAN_POINT('Origin',(0.,50.,0.));
#5806=CARTESIAN_POINT('Origin',(0.,50.,0.));
#5807=CARTESIAN_POINT('',(-1.52965876864867E-15,50.5625,-6.));
#5808=CARTESIAN_POINT('',(2.0935010245251E-14,50.506249998771,-6.));
#5809=CARTESIAN_POINT('',(-7.34788079488412E-16,50.,-6.));
#5810=CARTESIAN_POINT('Ctrl Pts',(1.11022302462516E-15,50.5625,-6.));
#5811=CARTESIAN_POINT('Ctrl Pts',(0.476472672014833,50.5565440915998,-6.));
#5812=CARTESIAN_POINT('Ctrl Pts',(0.952342916136355,50.5505957135482,-5.94324142107436));
#5813=CARTESIAN_POINT('Ctrl Pts',(2.15487129319964,50.535564108835,-5.65088635606439));
#5814=CARTESIAN_POINT('Ctrl Pts',(2.85164975918806,50.5274118357436,-5.33329821377427));
#5815=CARTESIAN_POINT('Ctrl Pts',(4.11877626853935,50.5097650355555,-4.4347324708146));
#5816=CARTESIAN_POINT('Ctrl Pts',(4.66914406878105,50.5000062126512,-3.85100602351549));
#5817=CARTESIAN_POINT('Ctrl Pts',(5.49975183061805,50.4804099614397,-2.52033349247185));
#5818=CARTESIAN_POINT('Ctrl Pts',(5.77873402031905,50.4707647501893,-1.79041748490187));
#5819=CARTESIAN_POINT('Ctrl Pts',(6.04305617758452,50.4526536893107,-0.269995813782789));
#5820=CARTESIAN_POINT('Ctrl Pts',(6.02788606094672,50.4446968849474,0.505980809288367));
#5821=CARTESIAN_POINT('Ctrl Pts',(5.69985850262359,50.4260858043139,2.03581199638024));
#5822=CARTESIAN_POINT('Ctrl Pts',(5.38000634383492,50.4161085580272,2.77280379910834));
#5823=CARTESIAN_POINT('Ctrl Pts',(4.48867993903998,50.3966646970468,4.05434319874371));
#5824=CARTESIAN_POINT('Ctrl Pts',(3.93535378351657,50.3873713829251,4.59335977946739));
#5825=CARTESIAN_POINT('Ctrl Pts',(2.63192129548323,50.369950097055,5.45013213550946));
#5826=CARTESIAN_POINT('Ctrl Pts',(1.88806980464463,50.361100872558,5.75031863985159));
#5827=CARTESIAN_POINT('Ctrl Pts',(0.335271683604976,50.341690896045,6.04191731940555));
#5828=CARTESIAN_POINT('Ctrl Pts',(-0.457848446331719,50.3317768944208,6.03386671313742));
#5829=CARTESIAN_POINT('Ctrl Pts',(-1.9694640440123,50.3128816994498,5.71810678616551));
#5830=CARTESIAN_POINT('Ctrl Pts',(-2.67595066180082,50.3044868675681,5.42354152179471));
#5831=CARTESIAN_POINT('Ctrl Pts',(-3.97145719940011,50.2871188781581,4.5671164322292));
#5832=CARTESIAN_POINT('Ctrl Pts',(-4.54056698419253,50.2774420154712,4.0017818353245));
#5833=CARTESIAN_POINT('Ctrl Pts',(-5.4156177211193,50.2578490970685,2.69707633960295));
#5834=CARTESIAN_POINT('Ctrl Pts',(-5.71889044460288,50.2481281972586,1.97419266862997));
#5835=CARTESIAN_POINT('Ctrl Pts',(-6.03066858894288,50.2298384149222,0.464660143335277));
#5836=CARTESIAN_POINT('Ctrl Pts',(-6.04074643451833,50.2219311981155,-0.30700873998632));
#5837=CARTESIAN_POINT('Ctrl Pts',(-5.76467205805915,50.2035512699327,-1.84548216186661));
#5838=CARTESIAN_POINT('Ctrl Pts',(-5.46827631697157,50.1935825943994,-2.5952248013838));
#5839=CARTESIAN_POINT('Ctrl Pts',(-4.61606755786416,50.1740325956351,-3.90915337278197));
#5840=CARTESIAN_POINT('Ctrl Pts',(-4.0784439382076,50.1646314228256,-4.46719937561014));
#5841=CARTESIAN_POINT('Ctrl Pts',(-2.80731661670282,50.1470149884145,-5.36065017826871));
#5842=CARTESIAN_POINT('Ctrl Pts',(-2.08181074478282,50.1385226343097,-5.68187235150351));
#5843=CARTESIAN_POINT('Ctrl Pts',(-0.882392025536312,50.1235299003191,-5.95130335519231));
#5844=CARTESIAN_POINT('Ctrl Pts',(-0.441341940389351,50.1180167742549,-6.));
#5845=CARTESIAN_POINT('Ctrl Pts',(9.71445146547012E-16,50.1125,-6.));
#5846=CARTESIAN_POINT('Origin',(0.,50.,0.));
#5847=CARTESIAN_POINT('',(6.,50.393749998771,0.));
#5848=CARTESIAN_POINT('',(6.,50.1968749993855,0.));
#5849=CARTESIAN_POINT('Ctrl Pts',(6.,50.393749998771,0.));
#5850=CARTESIAN_POINT('Ctrl Pts',(6.,50.3988676934681,-0.472752385765871));
#5851=CARTESIAN_POINT('Ctrl Pts',(5.94412631061322,50.4043166770945,-0.943849242317885));
#5852=CARTESIAN_POINT('Ctrl Pts',(5.71905899328923,50.4158503124434,-1.87933816182198));
#5853=CARTESIAN_POINT('Ctrl Pts',(5.54677711349615,50.4219074269274,-2.33940344059781));
#5854=CARTESIAN_POINT('Ctrl Pts',(4.95121361381124,50.437998009178,-3.48193901273638));
#5855=CARTESIAN_POINT('Ctrl Pts',(4.4440452275349,50.4479625421736,-4.10960933757635));
#5856=CARTESIAN_POINT('Ctrl Pts',(3.24080528215491,50.466278937471,-5.10691455209658));
#5857=CARTESIAN_POINT('Ctrl Pts',(2.56504807180657,50.4741868978735,-5.4775838590699));
#5858=CARTESIAN_POINT('Ctrl Pts',(1.24316375970988,50.4907104517747,-5.9029624523061));
#5859=CARTESIAN_POINT('Ctrl Pts',(0.622991567293922,50.4984626041798,-6.));
#5860=CARTESIAN_POINT('Ctrl Pts',(3.63598040564739E-14,50.506249998771,
-6.));
#5861=CARTESIAN_POINT('Origin',(0.,50.,0.));
#5862=CARTESIAN_POINT('',(5.8776104737723E-15,51.0125,-6.));
#5863=CARTESIAN_POINT('',(3.65716442452199E-15,50.956249998771,-6.));
#5864=CARTESIAN_POINT('',(-7.34788079488412E-16,50.,-6.));
#5865=CARTESIAN_POINT('Ctrl Pts',(1.58206781009085E-14,51.0125,-6.));
#5866=CARTESIAN_POINT('Ctrl Pts',(0.601653563824407,51.0049793304522,-6.));
#5867=CARTESIAN_POINT('Ctrl Pts',(1.20092291143887,50.9974884636069,-5.90949606770874));
#5868=CARTESIAN_POINT('Ctrl Pts',(2.50594358432149,50.9811757051959,-5.5047255931851));
#5869=CARTESIAN_POINT('Ctrl Pts',(3.1847068740602,50.9732585574772,-5.14192541668118));
#5870=CARTESIAN_POINT('Ctrl Pts',(4.39882179499044,50.9550207007929,-4.15815395852777));
#5871=CARTESIAN_POINT('Ctrl Pts',(4.91338690974145,50.9450623040753,-3.53532098195299));
#5872=CARTESIAN_POINT('Ctrl Pts',(5.65350068693484,50.9254580943553,-2.15166654899081));
#5873=CARTESIAN_POINT('Ctrl Pts',(5.88251857425753,50.9159965307216,-1.40986827814802));
#5874=CARTESIAN_POINT('Ctrl Pts',(6.04922997596698,50.8982658107267,0.131774603112445));
#5875=CARTESIAN_POINT('Ctrl Pts',(5.98068299604821,50.8899459720277,0.91759864356742));
#5876=CARTESIAN_POINT('Ctrl Pts',(5.5438020044826,50.8708757505391,2.42699688707256));
#5877=CARTESIAN_POINT('Ctrl Pts',(5.17645209976913,50.8609151616119,3.13502711244388));
#5878=CARTESIAN_POINT('Ctrl Pts',(4.20694003529658,50.8417559174161,4.34513422806219));
#5879=CARTESIAN_POINT('Ctrl Pts',(3.62280363610034,50.8327850454512,4.84291099325534));
#5880=CARTESIAN_POINT('Ctrl Pts',(2.27059691795816,50.8158824614744,5.61026834862654));
#5881=CARTESIAN_POINT('Ctrl Pts',(1.50889267209935,50.8063611584012,5.86122364397982));
#5882=CARTESIAN_POINT('Ctrl Pts',(-0.054498498555203,50.786818768768,6.05032206138634));
#5883=CARTESIAN_POINT('Ctrl Pts',(-0.840368151589543,50.7769953981051,5.99192403302677));
#5884=CARTESIAN_POINT('Ctrl Pts',(-2.32593591816436,50.7584258010229,5.58283012690718));
#5885=CARTESIAN_POINT('Ctrl Pts',(-3.01389064873413,50.7504258757977,5.24351291353162));
#5886=CARTESIAN_POINT('Ctrl Pts',(-4.26025821447966,50.732427877307,4.30051967936572));
#5887=CARTESIAN_POINT('Ctrl Pts',(-4.79671255812451,50.7224948600111,3.69266890552999));
#5888=CARTESIAN_POINT('Ctrl Pts',(-5.58313950087653,50.702816769394,2.32892856624056));
#5889=CARTESIAN_POINT('Ctrl Pts',(-5.83606608898751,50.6932626947642,1.59238819047398));
#5890=CARTESIAN_POINT('Ctrl Pts',(-6.04952440528675,50.675347728897,0.0607147482980532));
#5891=CARTESIAN_POINT('Ctrl Pts',(-6.00680377993718,50.667245707192,-0.720239050576822));
#5892=CARTESIAN_POINT('Ctrl Pts',(-5.62238021193402,50.6483922983037,-2.23989531159852));
#5893=CARTESIAN_POINT('Ctrl Pts',(-5.27762720706178,50.6384178537405,-2.96225179199993));
#5894=CARTESIAN_POINT('Ctrl Pts',(-4.34514342194628,50.6191112625712,-4.20734852504976));
#5895=CARTESIAN_POINT('Ctrl Pts',(-3.77550374701531,50.6099449611129,-4.72521356370631));
#5896=CARTESIAN_POINT('Ctrl Pts',(-2.44599834298937,50.5928577967403,-5.53606789283227));
#5897=CARTESIAN_POINT('Ctrl Pts',(-1.69240519125137,50.5836550648906,-5.81091707152203));
#5898=CARTESIAN_POINT('Ctrl Pts',(-0.606296241288776,50.5700787030161,-5.97704427499298));
#5899=CARTESIAN_POINT('Ctrl Pts',(-0.303026289114533,50.5662878286139,-6.));
#5900=CARTESIAN_POINT('Ctrl Pts',(4.85722573273506E-16,50.5625,-6.));
#5901=CARTESIAN_POINT('Ctrl Pts',(3.5978164891759E-14,50.506249998771,-6.));
#5902=CARTESIAN_POINT('Ctrl Pts',(-0.152003403865639,50.5081500413193,-6.));
#5903=CARTESIAN_POINT('Ctrl Pts',(-0.304174647594184,50.510052181866,-5.99422385574095));
#5904=CARTESIAN_POINT('Ctrl Pts',(-1.2482173623285,50.5218527158001,-5.92223895805082));
#5905=CARTESIAN_POINT('Ctrl Pts',(-2.02043362015721,50.531505419023,-5.70515799936607));
#5906=CARTESIAN_POINT('Ctrl Pts',(-3.40371495283626,50.5487964356815,-4.99904116312216));
#5907=CARTESIAN_POINT('Ctrl Pts',(-4.00797797076151,50.5572720195484,-4.52899800173635));
#5908=CARTESIAN_POINT('Ctrl Pts',(-5.02743121692379,50.5762120737144,-3.36797234844005));
#5909=CARTESIAN_POINT('Ctrl Pts',(-5.42507403926348,50.5861358260319,-2.6808345674558));
#5910=CARTESIAN_POINT('Ctrl Pts',(-5.93450499841088,50.605491209983,-1.18698088734165));
#5911=CARTESIAN_POINT('Ctrl Pts',(-6.03919864626748,50.6142384889631,-0.394124075355784));
#5912=CARTESIAN_POINT('Ctrl Pts',(-5.93632777073841,50.6317114764584,1.16056884240303));
#5913=CARTESIAN_POINT('Ctrl Pts',(-5.73980587496678,50.6410339113833,1.90827652312679));
#5914=CARTESIAN_POINT('Ctrl Pts',(-5.06310523712295,50.6605074794676,3.31647439179314));
#5915=CARTESIAN_POINT('Ctrl Pts',(-4.57877433964754,50.6704835153468,3.95839253781037));
#5916=CARTESIAN_POINT('Ctrl Pts',(-3.40909054731109,50.6890347370683,4.99676374218396));
#5917=CARTESIAN_POINT('Ctrl Pts',(-2.74234841966966,50.6969706435252,5.39157404784597));
#5918=CARTESIAN_POINT('Ctrl Pts',(-1.28970228179228,50.7151287202487,5.91075385984872));
#5919=CARTESIAN_POINT('Ctrl Pts',(-0.516435295961029,50.7247945575715,6.02773819372563));
#5920=CARTESIAN_POINT('Ctrl Pts',(1.05135832519143,50.7443919778359,5.96034931905182));
#5921=CARTESIAN_POINT('Ctrl Pts',(1.83043851808684,50.7541304802471,5.7689366459716));
#5922=CARTESIAN_POINT('Ctrl Pts',(3.23642006657542,50.7717052496032,5.10894082885421));
#5923=CARTESIAN_POINT('Ctrl Pts',(3.85590385180355,50.7799125840591,4.65915328260332));
#5924=CARTESIAN_POINT('Ctrl Pts',(4.911409365443,50.7986849582154,3.53443203143811));
#5925=CARTESIAN_POINT('Ctrl Pts',(5.33057380493307,50.8085687334406,2.86341268750622));
#5926=CARTESIAN_POINT('Ctrl Pts',(5.89333911364858,50.8281220796084,1.38206464221782));
#5927=CARTESIAN_POINT('Ctrl Pts',(6.02499747152435,50.8372730161237,0.583885731075924));
#5928=CARTESIAN_POINT('Ctrl Pts',(5.96852424689707,50.8545542654857,-0.979882872856363));
#5929=CARTESIAN_POINT('Ctrl Pts',(5.79544146966376,50.8637668988012,-1.7309800967731));
#5930=CARTESIAN_POINT('Ctrl Pts',(5.16480946229501,50.8831249119008,-3.15510118940353));
#5931=CARTESIAN_POINT('Ctrl Pts',(4.70262726478869,50.8931017932574,-3.80988499516316));
#5932=CARTESIAN_POINT('Ctrl Pts',(3.56553255119832,50.9118700954101,-4.88712454418799));
#5933=CARTESIAN_POINT('Ctrl Pts',(2.90721926588576,50.9199097579474,-5.30519385869809));
#5934=CARTESIAN_POINT('Ctrl Pts',(1.49047678297696,50.9376190389837,-5.8599679154867));
#5935=CARTESIAN_POINT('Ctrl Pts',(0.748406815975599,50.9468949135713,-6.));
#5936=CARTESIAN_POINT('Ctrl Pts',(8.74300631892311E-15,50.956249998771,
-6.));
#5937=CARTESIAN_POINT('Origin',(0.,50.,0.));
#5938=CARTESIAN_POINT('',(-6.44949795900495E-16,51.4625,-6.));
#5939=CARTESIAN_POINT('',(-3.06903603998188E-14,51.406249998771,-6.));
#5940=CARTESIAN_POINT('',(-7.34788079488412E-16,50.,-6.));
#5941=CARTESIAN_POINT('Ctrl Pts',(2.35922392732846E-15,51.4625,-6.));
#5942=CARTESIAN_POINT('Ctrl Pts',(0.729126527437651,51.453385918407,-6.));
#5943=CARTESIAN_POINT('Ctrl Pts',(1.45257389413295,51.4443428263233,-5.86708753239055));
#5944=CARTESIAN_POINT('Ctrl Pts',(2.85524232401819,51.4268094709497,-5.33310950763709));
#5945=CARTESIAN_POINT('Ctrl Pts',(3.51622153328107,51.4188108537407,-4.92246422249686));
#5946=CARTESIAN_POINT('Ctrl Pts',(4.66374479001418,51.4001108312203,-3.85755299791155));
#5947=CARTESIAN_POINT('Ctrl Pts',(5.13300751731751,51.3901331471364,-3.20678298515835));
#5948=CARTESIAN_POINT('Ctrl Pts',(5.77833250827751,51.3707364282851,-1.78756940637938));
#5949=CARTESIAN_POINT('Ctrl Pts',(5.95887574118884,51.3614879927408,-1.03747221033125));
#5950=CARTESIAN_POINT('Ctrl Pts',(6.03015613730497,51.3441451457851,0.5234376111266));
#5951=CARTESIAN_POINT('Ctrl Pts',(5.90716967249953,51.335131443154,1.31990283301873));
#5952=CARTESIAN_POINT('Ctrl Pts',(5.36147739674722,51.315640345333,2.80535774252139));
#5953=CARTESIAN_POINT('Ctrl Pts',(4.94913149322012,51.3057425956967,3.48160467082276));
#5954=CARTESIAN_POINT('Ctrl Pts',(3.90511006403264,51.286915968157,4.61796797412313));
#5955=CARTESIAN_POINT('Ctrl Pts',(3.29054200038651,51.2786317750047,5.0742320508147));
#5956=CARTESIAN_POINT('Ctrl Pts',(1.89181182918552,51.2611476478647,5.74909877162617));
#5957=CARTESIAN_POINT('Ctrl Pts',(1.11484561480856,51.251435570185,5.9487973907187));
#5958=CARTESIAN_POINT('Ctrl Pts',(-0.452903530529944,51.2318387058683,6.03294646757653));
#5959=CARTESIAN_POINT('Ctrl Pts',(-1.22816139551171,51.222147982556,5.92395084746659));
#5960=CARTESIAN_POINT('Ctrl Pts',(-2.68547298581604,51.2039315876772,5.41992639145892));
#5961=CARTESIAN_POINT('Ctrl Pts',(-3.35510942912662,51.1960138719864,5.03295221414885));
#5962=CARTESIAN_POINT('Ctrl Pts',(-4.53571663874673,51.177537843469,4.00783369833812));
#5963=CARTESIAN_POINT('Ctrl Pts',(-5.02748153880361,51.1675643401458,3.37044152321714));
#5964=CARTESIAN_POINT('Ctrl Pts',(-5.71971656360589,51.1480556848537,1.96797121961757));
#5965=CARTESIAN_POINT('Ctrl Pts',(-5.92417386032965,51.1386978639832,1.22157623114418));
#5966=CARTESIAN_POINT('Ctrl Pts',(-6.04267856970106,51.1211611102462,-0.329980961522083));
#5967=CARTESIAN_POINT('Ctrl Pts',(-5.94693589479211,51.1125322987399,-1.12108033315413));
#5968=CARTESIAN_POINT('Ctrl Pts',(-5.45536444033585,51.0932454615163,-2.61891312766104));
#5969=CARTESIAN_POINT('Ctrl Pts',(-5.06507198158196,51.0833107530727,-3.31130672661132));
#5970=CARTESIAN_POINT('Ctrl Pts',(-4.05781210853169,51.0643157595439,-4.48444730810267));
#5971=CARTESIAN_POINT('Ctrl Pts',(-3.45856108428655,51.0557320135535,-4.96129373331203));
#5972=CARTESIAN_POINT('Ctrl Pts',(-2.08291035391032,51.0385363794238,-5.68264072765549));
#5973=CARTESIAN_POINT('Ctrl Pts',(-1.3131598757117,51.0289144984463,-5.90817338077523));
#5974=CARTESIAN_POINT('Ctrl Pts',(-0.348046647051617,51.0168505830881,-5.99243780840527));
#5975=CARTESIAN_POINT('Ctrl Pts',(-0.17392370497713,51.0146740463122,-6.));
#5976=CARTESIAN_POINT('Ctrl Pts',(1.70696790036118E-14,51.0125,-6.));
#5977=CARTESIAN_POINT('Ctrl Pts',(8.92450088600247E-15,50.956249998771,
-6.));
#5978=CARTESIAN_POINT('Ctrl Pts',(-0.0236694939700509,50.9565458674456,
-6.));
#5979=CARTESIAN_POINT('Ctrl Pts',(-0.0473453262845365,50.9568418153495,
-5.99985993888696));
#5980=CARTESIAN_POINT('Ctrl Pts',(-0.865475177989564,50.9670684384958,-5.99017447353904));
#5981=CARTESIAN_POINT('Ctrl Pts',(-1.65020552722794,50.9768775678613,-5.82306397465396));
#5982=CARTESIAN_POINT('Ctrl Pts',(-3.07704855133587,50.9947131056627,-5.20663568267979));
#5983=CARTESIAN_POINT('Ctrl Pts',(-3.71098632648849,51.002746826765,-4.77554919943315));
#5984=CARTESIAN_POINT('Ctrl Pts',(-4.79939869161664,51.0213594783246,-3.68458126930465));
#5985=CARTESIAN_POINT('Ctrl Pts',(-5.2378834734425,51.0311967083489,-3.02901619171069));
#5986=CARTESIAN_POINT('Ctrl Pts',(-5.84386020371629,51.0507264147932,-1.57480001640781));
#5987=CARTESIAN_POINT('Ctrl Pts',(-6.00076345356614,51.0602111642092,-0.788342969138268));
#5988=CARTESIAN_POINT('Ctrl Pts',(-5.99926273157664,51.077057562383,0.766994191899727));
#5989=CARTESIAN_POINT('Ctrl Pts',(-5.85367677494241,51.0861313952624,1.52114487752692));
#5990=CARTESIAN_POINT('Ctrl Pts',(-5.27743730941944,51.105331307234,2.96206476222724));
#5991=CARTESIAN_POINT('Ctrl Pts',(-4.84159877308954,51.1152966396318,3.63099124074761));
#5992=CARTESIAN_POINT('Ctrl Pts',(-3.74344507819321,51.1343099694806,4.75334808640714));
#5993=CARTESIAN_POINT('Ctrl Pts',(-3.09486583810597,51.1425641757947,5.19899003599694));
#5994=CARTESIAN_POINT('Ctrl Pts',(-1.67246967653445,51.1603441278144,5.81339415782086));
#5995=CARTESIAN_POINT('Ctrl Pts',(-0.913518401626463,51.1698310187507,5.97981409959571));
#5996=CARTESIAN_POINT('Ctrl Pts',(0.656532155170128,51.1894566507107,6.01747330048976));
#5997=CARTESIAN_POINT('Ctrl Pts',(1.45274859455488,51.199409356203,5.87627039081847));
#5998=CARTESIAN_POINT('Ctrl Pts',(2.90675574161729,51.2175844455413,5.30390036844112));
#5999=CARTESIAN_POINT('Ctrl Pts',(3.55614425565295,51.2255153876614,4.8922826028945));
#6000=CARTESIAN_POINT('Ctrl Pts',(4.67836403780843,51.2439575069591,3.83658648965518));
#6001=CARTESIAN_POINT('Ctrl Pts',(5.13631558728198,51.2537367738425,3.19761496120145));
#6002=CARTESIAN_POINT('Ctrl Pts',(5.78886518522972,51.2733094150932,1.76632149606204));
#6003=CARTESIAN_POINT('Ctrl Pts',(5.97159814210816,51.2829059092566,0.985336259740639));
#6004=CARTESIAN_POINT('Ctrl Pts',(6.02117430454731,51.3000251205363,-0.567445928026152));
#6005=CARTESIAN_POINT('Ctrl Pts',(5.90112590328245,51.3087019176556,-1.32411411650511));
#6006=CARTESIAN_POINT('Ctrl Pts',(5.37550568819043,51.3277404092649,-2.77934766473404));
#6007=CARTESIAN_POINT('Ctrl Pts',(4.96446005702314,51.3376829976343,-3.46048733037337));
#6008=CARTESIAN_POINT('Ctrl Pts',(3.90324713248807,51.3569142092584,-4.62429899600857));
#6009=CARTESIAN_POINT('Ctrl Pts',(3.26364678912653,51.3654544139069,-5.09588808413548));
#6010=CARTESIAN_POINT('Ctrl Pts',(1.85663770964007,51.3830420274005,-5.75690279586834));
#6011=CARTESIAN_POINT('Ctrl Pts',(1.10578919839712,51.3924276337911,-5.94695282907335));
#6012=CARTESIAN_POINT('Ctrl Pts',(0.226339583391152,51.4034207539786,-5.99680138535396));
#6013=CARTESIAN_POINT('Ctrl Pts',(0.113113412960351,51.404836081109,-6.));
#6014=CARTESIAN_POINT('Ctrl Pts',(-7.18522463749593E-14,51.406249998771,
-6.));
#6015=CARTESIAN_POINT('Origin',(0.,50.,0.));
#6016=CARTESIAN_POINT('',(4.48983169299085E-15,51.9125,-6.));
#6017=CARTESIAN_POINT('',(-7.61853816932726E-15,51.856249998771,-6.));
#6018=CARTESIAN_POINT('',(-7.34788079488412E-16,50.,-6.));
#6019=CARTESIAN_POINT('Ctrl Pts',(1.57666182319377E-14,51.9125,-6.));
#6020=CARTESIAN_POINT('Ctrl Pts',(0.0924430517342845,51.9113444618533,-6.));
#6021=CARTESIAN_POINT('Ctrl Pts',(0.184967191480457,51.9101879101064,-5.99786359346722));
#6022=CARTESIAN_POINT('Ctrl Pts',(1.04490904993104,51.8994386368758,-5.95804877519037));
#6023=CARTESIAN_POINT('Ctrl Pts',(1.79840667952007,51.8900199165059,-5.77545917468654));
#6024=CARTESIAN_POINT('Ctrl Pts',(3.21034451142012,51.8723706936072,-5.12924978043591));
#6025=CARTESIAN_POINT('Ctrl Pts',(3.85280973532281,51.8639306708006,-4.66598152208977));
#6026=CARTESIAN_POINT('Ctrl Pts',(4.92589999521266,51.8447679633295,-3.51535538180445));
#6027=CARTESIAN_POINT('Ctrl Pts',(5.34489191970669,51.834816864418,-2.83801734055718));
#6028=CARTESIAN_POINT('Ctrl Pts',(5.88665914109795,51.8157260815796,-1.38727581393923));
#6029=CARTESIAN_POINT('Ctrl Pts',(6.0148587668374,51.8069285111895,-0.631449735032211));
#6030=CARTESIAN_POINT('Ctrl Pts',(5.98166780649966,51.7899022768464,0.922203612083062));
#6031=CARTESIAN_POINT('Ctrl Pts',(5.80720587787156,51.7803374787255,1.7050361738104));
#6032=CARTESIAN_POINT('Ctrl Pts',(5.16952332359099,51.7607764201622,3.14384316778836));
#6033=CARTESIAN_POINT('Ctrl Pts',(4.71775764789522,51.750977473331,3.78820406783819));
#6034=CARTESIAN_POINT('Ctrl Pts',(3.60636022497298,51.7324800640207,4.85525594567499));
#6035=CARTESIAN_POINT('Ctrl Pts',(2.96198649019483,51.7245248311274,5.27313724558066));
#6036=CARTESIAN_POINT('Ctrl Pts',(1.51407230849546,51.7064259038562,5.86088842016826));
#6037=CARTESIAN_POINT('Ctrl Pts',(0.718481536179256,51.6964810192022,6.01050736255478));
#6038=CARTESIAN_POINT('Ctrl Pts',(-0.853487612076338,51.676831404849,5.98877294558987));
#6039=CARTESIAN_POINT('Ctrl Pts',(-1.61481130609958,51.6673148586737,5.82977189026946));
#6040=CARTESIAN_POINT('Ctrl Pts',(-3.04190771790022,51.6494761535262,5.22983997346207));
#6041=CARTESIAN_POINT('Ctrl Pts',(-3.69325542961239,51.6412932439949,4.79210796388247));
#6042=CARTESIAN_POINT('Ctrl Pts',(-4.80261373614584,51.6223488062732,3.68258408586089));
#6043=CARTESIAN_POINT('Ctrl Pts',(-5.24601376188035,51.6123788015796,3.01759162709253));
#6044=CARTESIAN_POINT('Ctrl Pts',(-5.8378222397197,51.5931312744607,1.58126201695301));
#6045=CARTESIAN_POINT('Ctrl Pts',(-5.99125937980607,51.5840167139538,0.827881957130522));
#6046=CARTESIAN_POINT('Ctrl Pts',(-6.0083699018476,51.567064754705,-0.728194196054372));
#6047=CARTESIAN_POINT('Ctrl Pts',(-5.85933185788279,51.5577068077806,-1.51626187955861));
#6048=CARTESIAN_POINT('Ctrl Pts',(-5.26760096122616,51.5381929901524,-2.97723514477735));
#6049=CARTESIAN_POINT('Ctrl Pts',(-4.83513639153481,51.5283401250748,-3.63772029782657));
#6050=CARTESIAN_POINT('Ctrl Pts',(-3.7570404965506,51.5096767262397,-4.7393322772767));
#6051=CARTESIAN_POINT('Ctrl Pts',(-3.12769439993587,51.5015961799992,-5.17630593696793));
#6052=CARTESIAN_POINT('Ctrl Pts',(-1.70740286678856,51.4838425358348,-5.806547484345));
#6053=CARTESIAN_POINT('Ctrl Pts',(-0.924376327007982,51.4740547040876,-5.98136532622966));
#6054=CARTESIAN_POINT('Ctrl Pts',(-0.0867051686540407,51.4635838146081,
-5.99953035711345));
#6055=CARTESIAN_POINT('Ctrl Pts',(-0.0433425502532464,51.4630417818782,
-6.));
#6056=CARTESIAN_POINT('Ctrl Pts',(8.92450088600248E-16,51.4625,-6.));
#6057=CARTESIAN_POINT('Ctrl Pts',(-6.84174938925253E-14,51.406249998771,
-6.));
#6058=CARTESIAN_POINT('Ctrl Pts',(-0.682829483794224,51.4147853673184,-5.99999999999999));
#6059=CARTESIAN_POINT('Ctrl Pts',(-1.36154991554759,51.4232693727154,-5.88342572703261));
#6060=CARTESIAN_POINT('Ctrl Pts',(-2.72788892000143,51.440348610271,-5.3985522850297));
#6061=CARTESIAN_POINT('Ctrl Pts',(-3.39356269799421,51.4482580185231,-5.0069429255558));
#6062=CARTESIAN_POINT('Ctrl Pts',(-4.54997486002227,51.4665211913447,-3.98751815942739));
#6063=CARTESIAN_POINT('Ctrl Pts',(-5.02716012934551,51.4762312989628,-3.36603988357486));
#6064=CARTESIAN_POINT('Ctrl Pts',(-5.72633526724286,51.4958260731568,-1.95962113275784));
#6065=CARTESIAN_POINT('Ctrl Pts',(-5.93519982653713,51.5055159610265,-1.1850956430917));
#6066=CARTESIAN_POINT('Ctrl Pts',(-6.03676786753935,51.5229263324305,0.36456523978062));
#6067=CARTESIAN_POINT('Ctrl Pts',(-5.94237522903659,51.5312792187735,1.12413008956238));
#6068=CARTESIAN_POINT('Ctrl Pts',(-5.46740692741677,51.5501495145695,2.59307026996213));
#6069=CARTESIAN_POINT('Ctrl Pts',(-5.08150263678972,51.5600578002235,3.28555654622167));
#6070=CARTESIAN_POINT('Ctrl Pts',(-4.05814773950216,51.5794975557433,4.49049001396925));
#6071=CARTESIAN_POINT('Ctrl Pts',(-3.42757426035077,51.5884053205166,4.98846414670857));
#6072=CARTESIAN_POINT('Ctrl Pts',(-2.03615645946408,51.6057980430277,5.69556957119916));
#6073=CARTESIAN_POINT('Ctrl Pts',(-1.29399110079178,51.6150751100111,5.90855443995147));
#6074=CARTESIAN_POINT('Ctrl Pts',(0.260167210419777,51.6345020889012,6.04686735307427));
#6075=CARTESIAN_POINT('Ctrl Pts',(1.05837508521773,51.6444796873362,5.95920647898521));
#6076=CARTESIAN_POINT('Ctrl Pts',(2.54987339008844,51.6631234161471,5.48549489205059));
#6077=CARTESIAN_POINT('Ctrl Pts',(3.23185121945399,51.6710940591096,5.11347676787178));
#6078=CARTESIAN_POINT('Ctrl Pts',(4.42112424819284,51.6891792491168,4.12946558011599));
#6079=CARTESIAN_POINT('Ctrl Pts',(4.91630755110058,51.6988129017285,3.52544108476394));
#6080=CARTESIAN_POINT('Ctrl Pts',(5.65969707009764,51.7184079064646,2.14452822220431));
#6081=CARTESIAN_POINT('Ctrl Pts',(5.89362134311647,51.7281775430302,1.37710409603449));
#6082=CARTESIAN_POINT('Ctrl Pts',(6.04546282587192,51.7458635868776,-0.168996931216874));
#6083=CARTESIAN_POINT('Ctrl Pts',(5.97562959130781,51.7539881263655,-0.931687453613559));
#6084=CARTESIAN_POINT('Ctrl Pts',(5.54880763948184,51.7726930088022,-2.41314471042416));
#6085=CARTESIAN_POINT('Ctrl Pts',(5.18706468357243,51.7825580768145,-3.11558826504987));
#6086=CARTESIAN_POINT('Ctrl Pts',(4.20705474315048,51.8020573823026,-4.35104794574967));
#6087=CARTESIAN_POINT('Ctrl Pts',(3.59473708496763,51.8113157852089,-4.86916354403048));
#6088=CARTESIAN_POINT('Ctrl Pts',(2.23171010459133,51.8283536224636,-5.62147602523948));
#6089=CARTESIAN_POINT('Ctrl Pts',(1.49991165226443,51.8375011031177,-5.85933176219644));
#6090=CARTESIAN_POINT('Ctrl Pts',(0.496159456164859,51.8500480055689,-5.98463166999933));
#6091=CARTESIAN_POINT('Ctrl Pts',(0.247941674568198,51.8531507278389,-6.));
#6092=CARTESIAN_POINT('Ctrl Pts',(-1.17267306976032E-14,51.856249998771,
-6.));
#6093=CARTESIAN_POINT('Origin',(0.,50.,0.));
#6094=CARTESIAN_POINT('',(-9.45734505386267E-15,52.3625,-6.));
#6095=CARTESIAN_POINT('',(3.17965476092108E-14,52.306249998771,-6.));
#6096=CARTESIAN_POINT('',(-7.34788079488412E-16,50.,-6.));
#6097=CARTESIAN_POINT('Ctrl Pts',(-1.50573997714787E-14,52.3625,-6.));
#6098=CARTESIAN_POINT('Ctrl Pts',(0.218867784195469,52.3597641526975,-6.));
#6099=CARTESIAN_POINT('Ctrl Pts',(0.437994839314629,52.3570250645085,-5.98802456173197));
#6100=CARTESIAN_POINT('Ctrl Pts',(1.41543341424493,52.3448070823219,-5.88044745416016));
#6101=CARTESIAN_POINT('Ctrl Pts',(2.15159544557699,52.3356050569302,-5.65276652575058));
#6102=CARTESIAN_POINT('Ctrl Pts',(3.5326476238168,52.3183419047022,-4.9156222040165));
#6103=CARTESIAN_POINT('Ctrl Pts',(4.15722311421762,52.309149330625,-4.40005338233782));
#6104=CARTESIAN_POINT('Ctrl Pts',(5.15516415149115,52.2895779417722,-3.16828744922857));
#6105=CARTESIAN_POINT('Ctrl Pts',(5.5243713275488,52.2796984718593,-2.46882297352484));
#6106=CARTESIAN_POINT('Ctrl Pts',(5.96601865302547,52.260942102291,-0.991168972694993));
#6107=CARTESIAN_POINT('Ctrl Pts',(6.04343622383244,52.2527556742411,-0.229480366865192));
#6108=CARTESIAN_POINT('Ctrl Pts',(5.90716500607145,52.2351543708734,1.31778216686378));
#6109=CARTESIAN_POINT('Ctrl Pts',(5.6809768157088,52.2254083123868,2.08749467279664));
#6110=CARTESIAN_POINT('Ctrl Pts',(4.95118396568992,52.2058111553387,3.47645639791216));
#6111=CARTESIAN_POINT('Ctrl Pts',(4.46150970175715,52.1961528277785,4.08594091250292));
#6112=CARTESIAN_POINT('Ctrl Pts',(3.28239385516863,52.1780120002128,5.08095592961064));
#6113=CARTESIAN_POINT('Ctrl Pts',(2.60552540851252,52.1700690676063,5.45907142385025));
#6114=CARTESIAN_POINT('Ctrl Pts',(1.11966447758211,52.1514958059697,5.94810747115647));
#6115=CARTESIAN_POINT('Ctrl Pts',(0.321539219409664,52.1415192402425,6.04402472627572));
#6116=CARTESIAN_POINT('Ctrl Pts',(-1.23548602561916,52.1220564246797,5.92115850706941));
#6117=CARTESIAN_POINT('Ctrl Pts',(-1.98043099831077,52.112744612521,5.71528246658319));
#6118=CARTESIAN_POINT('Ctrl Pts',(-3.37675500006653,52.0952905624991,5.02256114425858));
#6119=CARTESIAN_POINT('Ctrl Pts',(-4.01016585633895,52.0865065480969,4.5329002576292));
#6120=CARTESIAN_POINT('Ctrl Pts',(-5.04548116745655,52.0671310648902,3.34080935998954));
#6121=CARTESIAN_POINT('Ctrl Pts',(-5.43929549024786,52.0572107945729,2.65178284716393));
#6122=CARTESIAN_POINT('Ctrl Pts',(-5.93013334981965,52.0382871396683,1.18707585699749));
#6123=CARTESIAN_POINT('Ctrl Pts',(-6.03258076592942,52.0298418558513,0.428460970690471));
#6124=CARTESIAN_POINT('Ctrl Pts',(-5.94739993750873,52.0125226070565,-1.12224352770716));
#6125=CARTESIAN_POINT('Ctrl Pts',(-5.74675091534023,52.0028609677718,-1.89890276744292));
#6126=CARTESIAN_POINT('Ctrl Pts',(-5.06217758730424,51.9832707673024,-3.31332937453221));
#6127=CARTESIAN_POINT('Ctrl Pts',(-4.59098826977479,51.9735377654933,-3.94038428954526));
#6128=CARTESIAN_POINT('Ctrl Pts',(-3.44532941940595,51.9552176218423,-4.97128022283922));
#6129=CARTESIAN_POINT('Ctrl Pts',(-2.78485079836899,51.9473106349795,-5.36922030587082));
#6130=CARTESIAN_POINT('Ctrl Pts',(-1.40463504649034,51.930057938081,-5.87584866556839));
#6131=CARTESIAN_POINT('Ctrl Pts',(-0.704673407088873,51.9213084175886,-6.));
#6132=CARTESIAN_POINT('Ctrl Pts',(1.67921232474555E-14,51.9125,-6.));
#6133=CARTESIAN_POINT('Ctrl Pts',(-1.37390099297363E-14,51.856249998771,
-6.));
#6134=CARTESIAN_POINT('Ctrl Pts',(-0.540992756444157,51.8630124082265,-5.99999999999999));
#6135=CARTESIAN_POINT('Ctrl Pts',(-1.08067101073368,51.8697583864051,-5.92682708894602));
#6136=CARTESIAN_POINT('Ctrl Pts',(-2.35171422551525,51.8856464265899,-5.57416455518408));
#6137=CARTESIAN_POINT('Ctrl Pts',(-3.05199153231469,51.8937765567516,-5.22371642671806));
#6138=CARTESIAN_POINT('Ctrl Pts',(-4.27665041483106,51.911663563064,-4.27844269669845));
#6139=CARTESIAN_POINT('Ctrl Pts',(-4.79062346986519,51.9212040079278,-3.69387663272464));
#6140=CARTESIAN_POINT('Ctrl Pts',(-5.58471546251296,51.9408720126469,-2.33549340740676));
#6141=CARTESIAN_POINT('Ctrl Pts',(-5.84660368323659,51.9508096095341,-1.56869876406795));
#6142=CARTESIAN_POINT('Ctrl Pts',(-6.04798129306953,51.9688448860489,-0.0189367011938789));
#6143=CARTESIAN_POINT('Ctrl Pts',(-6.00169394412353,51.9768266635303,0.747068330761391));
#6144=CARTESIAN_POINT('Ctrl Pts',(-5.62060806043904,51.9953697397694,2.23998430255282));
#6145=CARTESIAN_POINT('Ctrl Pts',(-5.28200909226598,52.0051843078803,2.95112506365597));
#6146=CARTESIAN_POINT('Ctrl Pts',(-4.343264457766,52.0247340310338,4.21506666426781));
#6147=CARTESIAN_POINT('Ctrl Pts',(-3.74781747966786,52.034271595978,4.75232770124426));
#6148=CARTESIAN_POINT('Ctrl Pts',(-2.4114876533685,52.0512199102857,5.54641552876093));
#6149=CARTESIAN_POINT('Ctrl Pts',(-1.68999863519737,52.0601250158311,5.80705970867361));
#6150=CARTESIAN_POINT('Ctrl Pts',(-0.15927307289999,52.0792590853598,6.0496282649839));
#6151=CARTESIAN_POINT('Ctrl Pts',(0.637312705374822,52.0892164075882,6.0180732298212));
#6152=CARTESIAN_POINT('Ctrl Pts',(2.16568132834483,52.1083210153754,5.64997174584619));
#6153=CARTESIAN_POINT('Ctrl Pts',(2.88330762224981,52.1166835593658,5.3196695424997));
#6154=CARTESIAN_POINT('Ctrl Pts',(4.14018966352825,52.1343841958284,4.4102159711343));
#6155=CARTESIAN_POINT('Ctrl Pts',(4.67069267170621,52.1438300751988,3.84392906614758));
#6156=CARTESIAN_POINT('Ctrl Pts',(5.5053081025277,52.1634206138229,2.51609807009338));
#6157=CARTESIAN_POINT('Ctrl Pts',(5.79121623205391,52.1733821090614,1.76096369244842));
#6158=CARTESIAN_POINT('Ctrl Pts',(6.04438646328482,52.1916578530666,0.218890678232439));
#6159=CARTESIAN_POINT('Ctrl Pts',(6.02320118561849,52.199569438352,-0.55097201213558));
#6160=CARTESIAN_POINT('Ctrl Pts',(5.69030954107534,52.2179373780415,-2.05553451942558));
#6161=CARTESIAN_POINT('Ctrl Pts',(5.3762506176683,52.2276889646437,-2.77502549942324));
#6162=CARTESIAN_POINT('Ctrl Pts',(4.48163229301664,52.2472735675887,-4.06766549402191));
#6163=CARTESIAN_POINT('Ctrl Pts',(3.90436395250857,52.2569104487973,-4.62459641582749));
#6164=CARTESIAN_POINT('Ctrl Pts',(2.59634506972209,52.2741521285476,-5.46212951296211));
#6165=CARTESIAN_POINT('Ctrl Pts',(1.88539609253017,52.2826825476144,-5.74640518100851));
#6166=CARTESIAN_POINT('Ctrl Pts',(0.763696519234804,52.2967037922806,-5.96355220594268));
#6167=CARTESIAN_POINT('Ctrl Pts',(0.38182666544753,52.3014771654529,-6.));
#6168=CARTESIAN_POINT('Ctrl Pts',(7.37604421985338E-14,52.306249998771,
-6.));
#6169=CARTESIAN_POINT('Origin',(0.,50.,0.));
#6170=CARTESIAN_POINT('',(-7.36700326531062E-15,52.8125,-6.));
#6171=CARTESIAN_POINT('',(3.06147672412016E-14,52.756249998771,-6.));
#6172=CARTESIAN_POINT('',(-7.34788079488412E-16,50.,-6.));
#6173=CARTESIAN_POINT('Ctrl Pts',(-1.14491749414469E-14,52.8125,-6.));
#6174=CARTESIAN_POINT('Ctrl Pts',(0.359533066415523,52.8080058366698,-6.));
#6175=CARTESIAN_POINT('Ctrl Pts',(0.719194283200083,52.80351007146,-5.96768432091232));
#6176=CARTESIAN_POINT('Ctrl Pts',(1.8215255466804,52.7897309306665,-5.76701278626887));
#6177=CARTESIAN_POINT('Ctrl Pts',(2.53589293275615,52.7810870945708,-5.49050179274652));
#6178=CARTESIAN_POINT('Ctrl Pts',(3.8532806219589,52.763941337833,-4.66723876685205));
#6179=CARTESIAN_POINT('Ctrl Pts',(4.43661013077627,52.7543359567424,-4.11671711846622));
#6180=CARTESIAN_POINT('Ctrl Pts',(5.34585807446428,52.7347604020581,-2.83335938087136));
#6181=CARTESIAN_POINT('Ctrl Pts',(5.66801918759594,52.7249869640751,-2.11652765819008));
#6182=CARTESIAN_POINT('Ctrl Pts',(6.01679524895255,52.7065607918979,-0.615756736438865));
#6183=CARTESIAN_POINT('Ctrl Pts',(6.04629083677593,52.6986352802673,0.152793435874327));
#6184=CARTESIAN_POINT('Ctrl Pts',(5.81026625134235,52.6804384052797,1.69747988554611));
#6185=CARTESIAN_POINT('Ctrl Pts',(5.53226434062804,52.6704836463375,2.4565566483534));
#6186=CARTESIAN_POINT('Ctrl Pts',(4.71095261061875,52.650865278049,3.79463933393641));
#6187=CARTESIAN_POINT('Ctrl Pts',(4.18585693462298,52.6413870859433,4.36703308622835));
#6188=CARTESIAN_POINT('Ctrl Pts',(2.93964037161027,52.6236241371035,5.2884005451934));
#6189=CARTESIAN_POINT('Ctrl Pts',(2.22782920664847,52.6153478650831,5.6254289134476));
#6190=CARTESIAN_POINT('Ctrl Pts',(0.705184014040115,52.5963148001755,6.01061589201909));
#6191=CARTESIAN_POINT('Ctrl Pts',(-0.0919183126728877,52.5863510210915,
6.0511433036594));
#6192=CARTESIAN_POINT('Ctrl Pts',(-1.62680507903547,52.567164936512,5.82517162440524));
#6193=CARTESIAN_POINT('Ctrl Pts',(-2.35175733075434,52.558121280367,5.57210108808757));
#6194=CARTESIAN_POINT('Ctrl Pts',(-3.69702974916344,52.5412677989699,4.79193655757096));
#6195=CARTESIAN_POINT('Ctrl Pts',(-4.29812828883109,52.5317641831702,4.26107453881697));
#6196=CARTESIAN_POINT('Ctrl Pts',(-5.25074960954657,52.5122302217109,3.00660064967072));
#6197=CARTESIAN_POINT('Ctrl Pts',(-5.59713037946457,52.5023976972256,2.29829397508418));
#6198=CARTESIAN_POINT('Ctrl Pts',(-5.99355862748471,52.4837998524007,0.809176616231353));
#6199=CARTESIAN_POINT('Ctrl Pts',(-6.04777158221044,52.4757783631922,0.0443211759275311));
#6200=CARTESIAN_POINT('Ctrl Pts',(-5.86375666606749,52.4579190949642,-1.49920629374432));
#6201=CARTESIAN_POINT('Ctrl Pts',(-5.61392726074293,52.4481039489542,-2.26165156988438));
#6202=CARTESIAN_POINT('Ctrl Pts',(-4.84273245148255,52.4285196980954,-3.62551764000003));
#6203=CARTESIAN_POINT('Ctrl Pts',(-4.33635602695557,52.4189398292719,-4.21811145002904));
#6204=CARTESIAN_POINT('Ctrl Pts',(-3.12614981265986,52.4009710618933,-5.17928219571708));
#6205=CARTESIAN_POINT('Ctrl Pts',(-2.43344099399138,52.3929180124248,-5.53860495466283));
#6206=CARTESIAN_POINT('Ctrl Pts',(-1.14120183459968,52.3767650229324,-5.91834520388219));
#6207=CARTESIAN_POINT('Ctrl Pts',(-0.571484748699384,52.3696435593587,-6.));
#6208=CARTESIAN_POINT('Ctrl Pts',(-1.346145417358E-14,52.3625,-6.));
#6209=CARTESIAN_POINT('Ctrl Pts',(7.28583859910259E-14,52.306249998771,
-6.));
#6210=CARTESIAN_POINT('Ctrl Pts',(-0.401217509922084,52.311265217645,-6.));
#6211=CARTESIAN_POINT('Ctrl Pts',(-0.802387333529942,52.3162798404401,-5.95975596723063));
#6212=CARTESIAN_POINT('Ctrl Pts',(-1.97205889691975,52.3309007349825,-5.72153419859104));
#6213=CARTESIAN_POINT('Ctrl Pts',(-2.70793242061734,52.3395856471272,-5.41221345393983));
#6214=CARTESIAN_POINT('Ctrl Pts',(-3.99745874815731,52.357091658676,-4.53958574945196));
#6215=CARTESIAN_POINT('Ctrl Pts',(-4.54410268846408,52.3664324944465,-3.99232132808627));
#6216=CARTESIAN_POINT('Ctrl Pts',(-5.41872646934361,52.3859244514314,-2.69669574545852));
#6217=CARTESIAN_POINT('Ctrl Pts',(-5.72853914181933,52.3958993209595,-1.9541271981608));
#6218=CARTESIAN_POINT('Ctrl Pts',(-6.03420119206698,52.4144117900263,-0.420492625292152));
#6219=CARTESIAN_POINT('Ctrl Pts',(-6.03849055947503,52.4223372120036,0.353595098947635));
#6220=CARTESIAN_POINT('Ctrl Pts',(-5.75381166082129,52.4405254457877,1.86939272759775));
#6221=CARTESIAN_POINT('Ctrl Pts',(-5.46440411634469,52.4502042499875,2.59639283751682));
#6222=CARTESIAN_POINT('Ctrl Pts',(-4.61465836409539,52.4698016634787,3.91612341143982));
#6223=CARTESIAN_POINT('Ctrl Pts',(-4.05618452379599,52.4795266716281,4.49204616107717));
#6224=CARTESIAN_POINT('Ctrl Pts',(-2.77683975502757,52.497054749469,5.37259058801151));
#6225=CARTESIAN_POINT('Ctrl Pts',(-2.07594967199261,52.5053006278711,5.68031825937686));
#6226=CARTESIAN_POINT('Ctrl Pts',(-0.571917507210461,52.5241010299309,6.02393082527088));
#6227=CARTESIAN_POINT('Ctrl Pts',(0.219371708102146,52.5339921451223,6.04704111370116));
#6228=CARTESIAN_POINT('Ctrl Pts',(1.78108360664636,52.5535135438541,5.78505138986634));
#6229=CARTESIAN_POINT('Ctrl Pts',(2.53515315850362,52.562592820824,5.4965487088559));
#6230=CARTESIAN_POINT('Ctrl Pts',(3.8560955030445,52.5799058428859,4.65988665539933));
#6231=CARTESIAN_POINT('Ctrl Pts',(4.41766562552434,52.5891370029495,4.13137127715813));
#6232=CARTESIAN_POINT('Ctrl Pts',(5.32972038187516,52.608515162003,2.86786868089532));
#6233=CARTESIAN_POINT('Ctrl Pts',(5.66208377876122,52.6184925812019,2.13808427191512));
#6234=CARTESIAN_POINT('Ctrl Pts',(6.01827497941694,52.6372258350133,0.613227496568188));
#6235=CARTESIAN_POINT('Ctrl Pts',(6.04718023195906,52.645243444225,-0.165198101203844));
#6236=CARTESIAN_POINT('Ctrl Pts',(5.80834075949411,52.6632568393674,-1.69131023299971));
#6237=CARTESIAN_POINT('Ctrl Pts',(5.54241375424038,52.6728576602113,-2.42466304471854));
#6238=CARTESIAN_POINT('Ctrl Pts',(4.7359041402153,52.6924470131212,-3.76861141008304));
#6239=CARTESIAN_POINT('Ctrl Pts',(4.19581736148071,52.702245316489,-4.36192065691855));
#6240=CARTESIAN_POINT('Ctrl Pts',(2.94408217595834,52.7200388305593,-5.28292543273532));
#6241=CARTESIAN_POINT('Ctrl Pts',(2.25234473625959,52.7280956895677,-5.61283098815292));
#6242=CARTESIAN_POINT('Ctrl Pts',(1.0209991201595,52.743487509769,-5.93471981245366));
#6243=CARTESIAN_POINT('Ctrl Pts',(0.510986821982903,52.7498626634962,-6.));
#6244=CARTESIAN_POINT('Ctrl Pts',(7.2997163869104E-14,52.756249998771,-6.));
#6245=CARTESIAN_POINT('Origin',(0.,50.,0.));
#6246=CARTESIAN_POINT('',(2.09176630104912E-14,53.2625,-6.));
#6247=CARTESIAN_POINT('',(-1.5563571689301E-14,53.206249998771,-6.));
#6248=CARTESIAN_POINT('',(-7.34788079488412E-16,50.,-6.));
#6249=CARTESIAN_POINT('Ctrl Pts',(3.24740234702858E-14,53.2625,-6.));
#6250=CARTESIAN_POINT('Ctrl Pts',(0.491259043487322,53.2563592619564,-6.));
#6251=CARTESIAN_POINT('Ctrl Pts',(0.981766247124528,53.2502279219108,-5.93966359261672));
#6252=CARTESIAN_POINT('Ctrl Pts',(2.19668792147501,53.2350414009815,-5.63479303766205));
#6253=CARTESIAN_POINT('Ctrl Pts',(2.89129907909015,53.2269328223526,-5.31194039765924));
#6254=CARTESIAN_POINT('Ctrl Pts',(4.15186450833354,53.2092230921359,-4.40377338630185));
#6255=CARTESIAN_POINT('Ctrl Pts',(4.69785860830518,53.1994470176055,-3.81592814502068));
#6256=CARTESIAN_POINT('Ctrl Pts',(5.51819126018113,53.179852975433,-2.47952733875372));
#6257=CARTESIAN_POINT('Ctrl Pts',(5.7915971879248,53.1702264099798,-1.7481142998087));
#6258=CARTESIAN_POINT('Ctrl Pts',(6.0450345184174,53.1521569235255,-0.225248751831639));
#6259=CARTESIAN_POINT('Ctrl Pts',(6.02401353226849,53.1441770784285,0.551762673190608));
#6260=CARTESIAN_POINT('Ctrl Pts',(5.68397847418228,53.1255136325642,2.07949861987119));
#6261=CARTESIAN_POINT('Ctrl Pts',(5.35877402192933,53.1155359284412,2.81344256764828));
#6262=CARTESIAN_POINT('Ctrl Pts',(4.45856813278751,53.0961193811304,4.08733226587911));
#6263=CARTESIAN_POINT('Ctrl Pts',(3.90170372579822,53.0868522527771,4.62188709850326));
#6264=CARTESIAN_POINT('Ctrl Pts',(2.59080580140653,53.0694769081903,5.47010540888669));
#6265=CARTESIAN_POINT('Ctrl Pts',(1.8426212209098,53.0605327652614,5.76533605389533));
#6266=CARTESIAN_POINT('Ctrl Pts',(0.286002065858915,53.0410750258232,6.0443673733577));
#6267=CARTESIAN_POINT('Ctrl Pts',(-0.506373489856741,53.0311703313768,6.02990557948782));
#6268=CARTESIAN_POINT('Ctrl Pts',(-2.0147821178542,53.0123152235268,5.70229239415533));
#6269=CARTESIAN_POINT('Ctrl Pts',(-2.71887969344214,53.0039869282711,5.40214419572939));
#6270=CARTESIAN_POINT('Ctrl Pts',(-4.00755213287817,52.9865508222372,4.53548109357146));
#6271=CARTESIAN_POINT('Ctrl Pts',(-4.57217721013319,52.976853122684,3.96563242230801));
#6272=CARTESIAN_POINT('Ctrl Pts',(-5.43653040942714,52.9572574539994,2.65449664019689));
#6273=CARTESIAN_POINT('Ctrl Pts',(-5.73393036442243,52.9475540224996,1.92983597811397));
#6274=CARTESIAN_POINT('Ctrl Pts',(-6.03422559788778,52.92930710304,0.417633294090379));
#6275=CARTESIAN_POINT('Ctrl Pts',(-6.03823131639805,52.9213954490686,-0.355047012897759));
#6276=CARTESIAN_POINT('Ctrl Pts',(-5.7496456227951,52.9029591903323,-1.89150061609016));
#6277=CARTESIAN_POINT('Ctrl Pts',(-5.44755803633235,52.8929874716582,-2.63823818045737));
#6278=CARTESIAN_POINT('Ctrl Pts',(-4.58582734675404,52.8734612376909,-3.94447396481805));
#6279=CARTESIAN_POINT('Ctrl Pts',(-4.04436465632552,52.8640852249845,-4.49797928833948));
#6280=CARTESIAN_POINT('Ctrl Pts',(-2.76545682823853,52.8465152547828,-5.38264583361932));
#6281=CARTESIAN_POINT('Ctrl Pts',(-2.03559289492947,52.8379449111866,-5.69885985218059));
#6282=CARTESIAN_POINT('Ctrl Pts',(-0.848661435065352,52.8231082679383,-5.95496633313774));
#6283=CARTESIAN_POINT('Ctrl Pts',(-0.424420007751195,52.8178052500969,-6.));
#6284=CARTESIAN_POINT('Ctrl Pts',(-1.56819002228303E-14,52.8125,-6.));
#6285=CARTESIAN_POINT('Ctrl Pts',(7.72992780895265E-14,52.756249998771,
-6.));
#6286=CARTESIAN_POINT('Ctrl Pts',(-0.267344232452943,52.7595918016766,-6.));
#6287=CARTESIAN_POINT('Ctrl Pts',(-0.534955221209766,52.7629369390361,-5.98213223044391));
#6288=CARTESIAN_POINT('Ctrl Pts',(-1.58812837821419,52.7761016034986,-5.84025745575398));
#6289=CARTESIAN_POINT('Ctrl Pts',(-2.34637786610327,52.7855204317038,-5.57899834959854));
#6290=CARTESIAN_POINT('Ctrl Pts',(-3.68892829615446,52.8024212061836,-4.79289353052493));
#6291=CARTESIAN_POINT('Ctrl Pts',(-4.26690007172733,52.8115160543365,-4.28643960604275));
#6292=CARTESIAN_POINT('Ctrl Pts',(-5.22063299391897,52.8307406542347,-3.06118509720213));
#6293=CARTESIAN_POINT('Ctrl Pts',(-5.57833851506736,52.8407085219569,-2.34691429810463));
#6294=CARTESIAN_POINT('Ctrl Pts',(-5.99267030213188,52.8596865961856,-0.833009464551543));
#6295=CARTESIAN_POINT('Ctrl Pts',(-6.05008800103878,52.8679032121247,-0.049304478823019));
#6296=CARTESIAN_POINT('Ctrl Pts',(-5.86334588471578,52.8857133464227,1.48810964304889));
#6297=CARTESIAN_POINT('Ctrl Pts',(-5.62409129279005,52.8952155505298,2.22775195585791));
#6298=CARTESIAN_POINT('Ctrl Pts',(-4.8641123352457,52.9148537207022,3.60307435380763));
#6299=CARTESIAN_POINT('Ctrl Pts',(-4.34013798093304,52.924802550029,4.2195911056831));
#6300=CARTESIAN_POINT('Ctrl Pts',(-3.11217506016,52.9429386857438,5.18597083674231));
#6301=CARTESIAN_POINT('Ctrl Pts',(-2.42951782408877,52.9508810259699,5.53871589289677));
#6302=CARTESIAN_POINT('Ctrl Pts',(-0.951878889039818,52.969351512658,5.97503535140572));
#6303=CARTESIAN_POINT('Ctrl Pts',(-0.168721490538011,52.9791409801393,6.04802840329404));
#6304=CARTESIAN_POINT('Ctrl Pts',(1.39663754809634,52.9987079681222,5.88899170824065));
#6305=CARTESIAN_POINT('Ctrl Pts',(2.16306991931943,53.0082883727625,5.65260725548448));
#6306=CARTESIAN_POINT('Ctrl Pts',(3.52880528145598,53.0253600647892,4.91166095187723));
#6307=CARTESIAN_POINT('Ctrl Pts',(4.12161405681198,53.0340975560578,4.42596998738146));
#6308=CARTESIAN_POINT('Ctrl Pts',(5.11296433136239,53.0531628596175,3.23714903247618));
#6309=CARTESIAN_POINT('Ctrl Pts',(5.49361928798084,53.0631099451367,2.5380478737987));
#6310=CARTESIAN_POINT('Ctrl Pts',(5.96202876101701,53.0823062579866,1.03520478653231));
#6311=CARTESIAN_POINT('Ctrl Pts',(6.0462161597879,53.0907942131497,0.246360867567393));
#6312=CARTESIAN_POINT('Ctrl Pts',(5.90735816387129,53.1084133504039,-1.30105561296681));
#6313=CARTESIAN_POINT('Ctrl Pts',(5.69254643262476,53.1178159762678,-2.04561137388686));
#6314=CARTESIAN_POINT('Ctrl Pts',(4.98008915095325,53.1373673273797,-3.44035042292738));
#6315=CARTESIAN_POINT('Ctrl Pts',(4.4786734245861,53.1473358060219,-4.07170653072655));
#6316=CARTESIAN_POINT('Ctrl Pts',(3.28388714913542,53.1657124321822,-5.07945636264507));
#6317=CARTESIAN_POINT('Ctrl Pts',(2.61043683240265,53.1736195383659,-5.45622691503375));
#6318=CARTESIAN_POINT('Ctrl Pts',(1.27568996261008,53.1903038742384,-5.89777164064974));
#6319=CARTESIAN_POINT('Ctrl Pts',(0.639437262180362,53.1982570329937,-6.00000000000001));
#6320=CARTESIAN_POINT('Ctrl Pts',(-4.08006961549745E-14,53.206249998771,
-6.));
#6321=CARTESIAN_POINT('Origin',(0.,50.,0.));
#6322=CARTESIAN_POINT('',(-5.50217552863555E-15,53.7125,-6.));
#6323=CARTESIAN_POINT('',(2.29472894773841E-14,53.656249998771,-6.));
#6324=CARTESIAN_POINT('',(-7.34788079488412E-16,50.,-6.));
#6325=CARTESIAN_POINT('Ctrl Pts',(-2.47024622979097E-14,53.7125,-6.));
#6326=CARTESIAN_POINT('Ctrl Pts',(0.618074665760965,53.704774066678,-6.));
#6327=CARTESIAN_POINT('Ctrl Pts',(1.23343403762461,53.6970820745296,-5.90448815830154));
#6328=CARTESIAN_POINT('Ctrl Pts',(2.55144973118435,53.6806068783601,-5.48389513563829));
#6329=CARTESIAN_POINT('Ctrl Pts',(3.22789828178359,53.6726976087109,-5.11504376016517));
#6330=CARTESIAN_POINT('Ctrl Pts',(4.43365342683385,53.6543992725919,-4.12085893228748));
#6331=CARTESIAN_POINT('Ctrl Pts',(4.94253298882412,53.6444360521858,-3.49429780703739));
#6332=CARTESIAN_POINT('Ctrl Pts',(5.67067377046189,53.6248539348408,-2.10577156805253));
#6333=CARTESIAN_POINT('Ctrl Pts',(5.89353510406379,53.6154175520843,-1.36274491905413));
#6334=CARTESIAN_POINT('Ctrl Pts',(6.04818455072785,53.597734988601,0.181413427204201));
#6335=CARTESIAN_POINT('Ctrl Pts',(5.97288847797361,53.5893458516483,0.968535222468236));
#6336=CARTESIAN_POINT('Ctrl Pts',(5.52237838947031,53.5702207243553,2.47513668414208));
#6337=CARTESIAN_POINT('Ctrl Pts',(5.14925095887713,53.5602654979815,3.17933588192937));
#6338=CARTESIAN_POINT('Ctrl Pts',(4.17027238796539,53.5411466073777,4.38024980235338));
#6339=CARTESIAN_POINT('Ctrl Pts',(3.58240017105194,53.532280002138,4.87279497735445));
#6340=CARTESIAN_POINT('Ctrl Pts',(2.22434107147549,53.5153042633933,5.62877258078118));
#6341=CARTESIAN_POINT('Ctrl Pts',(1.46056358190155,53.5057570447737,5.87345782879563));
#6342=CARTESIAN_POINT('Ctrl Pts',(-0.103746845680585,53.4862031644289,6.04959757139315));
#6343=CARTESIAN_POINT('Ctrl Pts',(-0.888479643857466,53.4763940044517,5.9848979741683));
#6344=CARTESIAN_POINT('Ctrl Pts',(-2.37064544174391,53.4578669319781,5.56406189814694));
#6345=CARTESIAN_POINT('Ctrl Pts',(-3.05631021084422,53.44989513097,5.21897575207413));
#6346=CARTESIAN_POINT('Ctrl Pts',(-4.29478343013108,53.4318374710426,4.26591342741277));
#6347=CARTESIAN_POINT('Ctrl Pts',(-4.82588893847439,53.4218972343699,3.65430760460912));
#6348=CARTESIAN_POINT('Ctrl Pts',(-5.60096633355719,53.4022355275788,2.28552807393122));
#6349=CARTESIAN_POINT('Ctrl Pts',(-5.84801981564352,53.3927033962653,1.54762389555455));
#6350=CARTESIAN_POINT('Ctrl Pts',(-6.05000568544818,53.3748332940483,0.0134711597906734));
#6351=CARTESIAN_POINT('Ctrl Pts',(-6.00099388817791,53.3666852976059,-0.768653128073082));
#6352=CARTESIAN_POINT('Ctrl Pts',(-5.6037508550172,53.3477781178544,-2.28587520700342));
#6353=CARTESIAN_POINT('Ctrl Pts',(-5.2534239545714,53.3378060616091,-3.0047929739411));
#6354=CARTESIAN_POINT('Ctrl Pts',(-4.31178217448903,53.3185338396968,-4.24142744016629));
#6355=CARTESIAN_POINT('Ctrl Pts',(-3.73854364388895,53.3093978219124,-4.7544171925566));
#6356=CARTESIAN_POINT('Ctrl Pts',(-2.40339227005806,53.2923899449371,-5.55468756347263));
#6357=CARTESIAN_POINT('Ctrl Pts',(-1.64777511202965,53.2830971889003,-5.82372103007885));
#6358=CARTESIAN_POINT('Ctrl Pts',(-0.575720817653312,53.2696965102206,-5.97930315353356));
#6359=CARTESIAN_POINT('Ctrl Pts',(-0.287731450645414,53.2660966431331,-6.));
#6360=CARTESIAN_POINT('Ctrl Pts',(3.35148575558719E-14,53.2625,-6.));
#6361=CARTESIAN_POINT('Ctrl Pts',(-4.25007251614318E-14,53.206249998771,
-6.));
#6362=CARTESIAN_POINT('Ctrl Pts',(-0.135125960113356,53.2079390732724,-6.));
#6363=CARTESIAN_POINT('Ctrl Pts',(-0.270394130633584,53.2096299254039,-5.99543532220098));
#6364=CARTESIAN_POINT('Ctrl Pts',(-1.19811557297958,53.2212264434332,-5.93258149174789));
#6365=CARTESIAN_POINT('Ctrl Pts',(-1.9721655079933,53.2309020676209,-5.72202636460942));
#6366=CARTESIAN_POINT('Ctrl Pts',(-3.36128493091421,53.2482660604074,-5.02765194059061));
#6367=CARTESIAN_POINT('Ctrl Pts',(-3.96941649553547,53.2566649403245,-4.5628141001609));
#6368=CARTESIAN_POINT('Ctrl Pts',(-4.99817162713518,53.2755624759913,-3.41108658364329));
#6369=CARTESIAN_POINT('Ctrl Pts',(-5.40139887038662,53.2854770039046,-2.72802508353873));
#6370=CARTESIAN_POINT('Ctrl Pts',(-5.92451595308842,53.3048841619358,-1.23729040588996));
#6371=CARTESIAN_POINT('Ctrl Pts',(-6.03609454420458,53.3137279541916,-0.443077411548285));
#6372=CARTESIAN_POINT('Ctrl Pts',(-5.945170224019,53.3311519300301,1.11398535022657));
#6373=CARTESIAN_POINT('Ctrl Pts',(-5.7547002884681,53.3404467684839,1.86263787900088));
#6374=CARTESIAN_POINT('Ctrl Pts',(-5.08986823307635,53.359892202276,3.27508914235736));
#6375=CARTESIAN_POINT('Ctrl Pts',(-4.61122888937136,53.3698694038797,3.92040099349111));
#6376=CARTESIAN_POINT('Ctrl Pts',(-3.44991154057133,53.3884773944313,4.96884664619351));
#6377=CARTESIAN_POINT('Ctrl Pts',(-2.78536159854707,53.3964329787891,5.36964488468559));
#6378=CARTESIAN_POINT('Ctrl Pts',(-1.33628151113567,53.4145464798818,5.90031898118643));
#6379=CARTESIAN_POINT('Ctrl Pts',(-0.564577998719876,53.4241927737871,6.0233423886157));
#6380=CARTESIAN_POINT('Ctrl Pts',(1.00312974829782,53.4437891206248,5.96865836317032));
#6381=CARTESIAN_POINT('Ctrl Pts',(1.78375291069941,53.4535469101548,5.78354509277361));
#6382=CARTESIAN_POINT('Ctrl Pts',(3.19519965664455,53.4711899944791,5.13484739601032));
#6383=CARTESIAN_POINT('Ctrl Pts',(3.81842392657344,53.4793449766578,4.68994756343085));
#6384=CARTESIAN_POINT('Ctrl Pts',(4.88256744925791,53.4980760320153,3.57403033625501));
#6385=CARTESIAN_POINT('Ctrl Pts',(5.30683580462029,53.5079485253874,2.90699991247375));
#6386=CARTESIAN_POINT('Ctrl Pts',(5.8792561253982,53.5274379477346,1.43713122060551));
#6387=CARTESIAN_POINT('Ctrl Pts',(6.01766909512581,53.5366354886232,0.647009039018205));
#6388=CARTESIAN_POINT('Ctrl Pts',(5.97949354956766,53.5537273034523,-0.909824522287626));
#6389=CARTESIAN_POINT('Ctrl Pts',(5.81547375410483,53.562895375946,-1.66203790876649));
#6390=CARTESIAN_POINT('Ctrl Pts',(5.20272810110748,53.5822039590112,-3.09191954192257));
#6391=CARTESIAN_POINT('Ctrl Pts',(4.74918591129041,53.5921785242975,-3.75147770904066));
#6392=CARTESIAN_POINT('Ctrl Pts',(3.62483532752884,53.6110287442997,-4.8436423316542));
#6393=CARTESIAN_POINT('Ctrl Pts',(2.96974381172352,53.6191282011245,-5.27076083695245));
#6394=CARTESIAN_POINT('Ctrl Pts',(1.53633499263769,53.6370458113631,-5.85107641045857));
#6395=CARTESIAN_POINT('Ctrl Pts',(0.771906526198351,53.6466011671936,-5.99996400996191));
#6396=CARTESIAN_POINT('Ctrl Pts',(0.000186533161219277,53.6562476671065,
-5.99999999782549));
#6397=CARTESIAN_POINT('Ctrl Pts',(9.32665259702794E-5,53.6562488329394,
-6.));
#6398=CARTESIAN_POINT('Ctrl Pts',(3.03433030124084E-14,53.656249998771,
-6.));
#6399=CARTESIAN_POINT('Origin',(0.,50.,0.));
#6400=CARTESIAN_POINT('',(1.71880075371411E-14,54.1625,-6.));
#6401=CARTESIAN_POINT('',(2.22534000869934E-14,54.106249998771,-6.));
#6402=CARTESIAN_POINT('',(-7.34788079488412E-16,50.,-6.));
#6403=CARTESIAN_POINT('Ctrl Pts',(3.40005801291454E-14,54.1625,-6.));
#6404=CARTESIAN_POINT('Ctrl Pts',(0.744020055647716,54.1531997493044,-6.));
#6405=CARTESIAN_POINT('Ctrl Pts',(1.48185695652323,54.1439767880434,-5.86160406932495));
#6406=CARTESIAN_POINT('Ctrl Pts',(2.89541452330477,54.1263073184586,-5.31158997658908));
#6407=CARTESIAN_POINT('Ctrl Pts',(3.55433416718244,54.1182776625721,-4.89521447158238));
#6408=CARTESIAN_POINT('Ctrl Pts',(4.69381032287955,54.0995248539421,-3.82078107911201));
#6409=CARTESIAN_POINT('Ctrl Pts',(5.15760866923583,54.0895477018416,-3.16690534707895));
#6410=CARTESIAN_POINT('Ctrl Pts',(5.79159158877462,54.0701807100565,-1.74388948905437));
#6411=CARTESIAN_POINT('Ctrl Pts',(5.96637457395195,54.0609598476221,-0.993013707211756));
#6412=CARTESIAN_POINT('Ctrl Pts',(6.0262257916751,54.0436645121126,0.570105834070089));
#6413=CARTESIAN_POINT('Ctrl Pts',(5.89655136082426,54.0345455731147,1.36789270390674));
#6414=CARTESIAN_POINT('Ctrl Pts',(5.33768512386391,54.0150063481362,2.85018741973248));
#6415=CARTESIAN_POINT('Ctrl Pts',(4.92007193606728,54.0051192842995,3.52240616815637));
#6416=CARTESIAN_POINT('Ctrl Pts',(3.86718457237685,53.9863344729565,4.64978790699034));
#6417=CARTESIAN_POINT('Ctrl Pts',(3.24882717012052,53.9781103396264,5.10105410207349));
#6418=CARTESIAN_POINT('Ctrl Pts',(1.84450031310309,53.9605562539137,5.7644551725158));
#6419=CARTESIAN_POINT('Ctrl Pts',(1.06589585930534,53.9508236982412,5.9577658430625));
#6420=CARTESIAN_POINT('Ctrl Pts',(-0.501903416108012,53.9312262072986,6.02898893194592));
#6421=CARTESIAN_POINT('Ctrl Pts',(-1.27563304331206,53.9215545869585,5.91382995961615));
#6422=CARTESIAN_POINT('Ctrl Pts',(-2.72935036690895,53.9033831204136,5.39811790017014));
#6423=CARTESIAN_POINT('Ctrl Pts',(-3.39675431349287,53.895452152632,5.00510648807065));
#6424=CARTESIAN_POINT('Ctrl Pts',(-4.56894829391694,53.8769181026692,3.96977080057932));
#6425=CARTESIAN_POINT('Ctrl Pts',(-5.05498728566334,53.8669425468884,3.32888317284369));
#6426=CARTESIAN_POINT('Ctrl Pts',(-5.73525397146423,53.8474607495571,1.92198397764554));
#6427=CARTESIAN_POINT('Ctrl Pts',(-5.93359607726064,53.8381301176553,1.1745699913819));
#6428=CARTESIAN_POINT('Ctrl Pts',(-6.04005597695363,53.8206424541455,-0.379406514454436));
#6429=CARTESIAN_POINT('Ctrl Pts',(-5.93742305258649,53.8119231582694,-1.17185807748706));
#6430=CARTESIAN_POINT('Ctrl Pts',(-5.43209720404327,53.79258343215,-2.66663543577941));
#6431=CARTESIAN_POINT('Ctrl Pts',(-5.03613761430514,53.78265705298,-3.35498768979131));
#6432=CARTESIAN_POINT('Ctrl Pts',(-4.01948150856907,53.7637043156959,-4.51879988913556));
#6433=CARTESIAN_POINT('Ctrl Pts',(-3.41637409273498,53.7552046761591,-4.99040568401792));
#6434=CARTESIAN_POINT('Ctrl Pts',(-2.03484549718193,53.7379355687147,-5.70003249367143));
#6435=CARTESIAN_POINT('Ctrl Pts',(-1.26318875578654,53.7282898594473,-5.91906256818622));
#6436=CARTESIAN_POINT('Ctrl Pts',(-0.314279853539542,53.7164284981692,-5.99383377292694));
#6437=CARTESIAN_POINT('Ctrl Pts',(-0.157052268400006,53.714463153355,-6.));
#6438=CARTESIAN_POINT('Ctrl Pts',(-2.15452655716319E-14,53.7125,-6.));
#6439=CARTESIAN_POINT('Ctrl Pts',(2.62290189567693E-14,53.656249998771,
-6.));
#6440=CARTESIAN_POINT('Ctrl Pts',(-0.802599966653911,53.6662824983541,-6.));
#6441=CARTESIAN_POINT('Ctrl Pts',(-1.59710684431166,53.6762138343249,-5.83895830100868));
#6442=CARTESIAN_POINT('Ctrl Pts',(-3.03657743603123,53.6942072167214,-5.2304033645235));
#6443=CARTESIAN_POINT('Ctrl Pts',(-3.67418475545865,53.7022089655309,-4.80398729501233));
#6444=CARTESIAN_POINT('Ctrl Pts',(-4.77075168658479,53.7207810741442,-3.72147260271503));
#6445=CARTESIAN_POINT('Ctrl Pts',(-5.21396967840967,53.7306052680037,-3.06984447450466));
#6446=CARTESIAN_POINT('Ctrl Pts',(-5.83120699784716,53.7501469341951,-1.62102480927238));
#6447=CARTESIAN_POINT('Ctrl Pts',(-5.99434172267899,53.7596666800625,-0.835814232303809));
#6448=CARTESIAN_POINT('Ctrl Pts',(-6.00513609416499,53.7765649148666,0.718945700488526));
#6449=CARTESIAN_POINT('Ctrl Pts',(-5.86573676047876,53.7855421431641,1.47367493621472));
#6450=CARTESIAN_POINT('Ctrl Pts',(-5.30175469450441,53.8047037726895,2.91813525294736));
#6451=CARTESIAN_POINT('Ctrl Pts',(-4.87188929188569,53.8146646574456,3.59009946627435));
#6452=CARTESIAN_POINT('Ctrl Pts',(-3.78260524830901,53.8337315976273,4.72252951793732));
#6453=CARTESIAN_POINT('Ctrl Pts',(-3.13620136273259,53.8420474817369,5.17441978277654));
#6454=CARTESIAN_POINT('Ctrl Pts',(-1.71751515098164,53.8597810593838,5.80016811140914));
#6455=CARTESIAN_POINT('Ctrl Pts',(-0.960471520801086,53.869244104761,5.97237712439266));
#6456=CARTESIAN_POINT('Ctrl Pts',(0.607967328528821,53.8888495903777,6.02248351713028));
#6457=CARTESIAN_POINT('Ctrl Pts',(1.4046143311556,53.8988076779105,5.88786911885732));
#6458=CARTESIAN_POINT('Ctrl Pts',(2.86335348217455,53.9170419172982,5.32755957371081));
#6459=CARTESIAN_POINT('Ctrl Pts',(3.51668660829516,53.9249597054766,4.92083344100594));
#6460=CARTESIAN_POINT('Ctrl Pts',(4.64732036441513,53.9433583882882,3.87400762861805));
#6461=CARTESIAN_POINT('Ctrl Pts',(5.11004964613728,53.9531216209987,3.23927569860641));
#6462=CARTESIAN_POINT('Ctrl Pts',(5.77412389849353,53.9727017559661,1.81394375589823));
#6463=CARTESIAN_POINT('Ctrl Pts',(5.96328856213595,53.9823221920229,1.03446020983009));
#6464=CARTESIAN_POINT('Ctrl Pts',(6.02562747346526,53.9995134266739,-0.517606635486794));
#6465=CARTESIAN_POINT('Ctrl Pts',(5.91190507370029,54.0081023759522,-1.27495418323414));
#6466=CARTESIAN_POINT('Ctrl Pts',(5.39880069617624,54.0270998861552,-2.73362805348819));
#6467=CARTESIAN_POINT('Ctrl Pts',(4.99393802567096,54.0370350698962,-3.41765344286178));
#6468=CARTESIAN_POINT('Ctrl Pts',(3.94199431913957,54.0563187217668,-4.59166091647857));
#6469=CARTESIAN_POINT('Ctrl Pts',(3.30461752451987,54.0649422797145,-5.06972942274412));
#6470=CARTESIAN_POINT('Ctrl Pts',(1.90144255569312,54.0824819668248,-5.74218208593506));
#6471=CARTESIAN_POINT('Ctrl Pts',(1.152687822376,54.0918414009913,-5.9379654414117));
#6472=CARTESIAN_POINT('Ctrl Pts',(0.258259320259502,54.1030217572678,-5.99583591381765));
#6473=CARTESIAN_POINT('Ctrl Pts',(0.129060583442295,54.1046367414779,-6.));
#6474=CARTESIAN_POINT('Ctrl Pts',(3.04270497686332E-14,54.106249998771,
-6.));
#6475=CARTESIAN_POINT('Origin',(0.,50.,0.));
#6476=CARTESIAN_POINT('',(-2.78454138992168E-14,54.6125,-6.));
#6477=CARTESIAN_POINT('',(9.65930765140174E-15,54.556249998771,-6.));
#6478=CARTESIAN_POINT('',(-7.34788079488412E-16,50.,-6.));
#6479=CARTESIAN_POINT('Ctrl Pts',(-1.90125692967058E-14,54.6125,-6.));
#6480=CARTESIAN_POINT('Ctrl Pts',(0.108463475076468,54.6111442065615,-6.));
#6481=CARTESIAN_POINT('Ctrl Pts',(0.217032411991259,54.6097870948501,-5.99705895880486));
#6482=CARTESIAN_POINT('Ctrl Pts',(1.09210248833924,54.5988487188957,-5.94950343388131));
#6483=CARTESIAN_POINT('Ctrl Pts',(1.84355332705342,54.5894555834118,-5.76112885167375));
#6484=CARTESIAN_POINT('Ctrl Pts',(3.25167517207667,54.571854060349,-5.10344666315784));
#6485=CARTESIAN_POINT('Ctrl Pts',(3.89192160881287,54.5633371643405,-4.63373699445241));
#6486=CARTESIAN_POINT('Ctrl Pts',(4.95581982341022,54.5441213118971,-3.47289450208802));
#6487=CARTESIAN_POINT('Ctrl Pts',(5.36865973088282,54.5341767025107,-2.79260406881144));
#6488=CARTESIAN_POINT('Ctrl Pts',(5.89791975275551,54.5151263660822,-1.33837778648844));
#6489=CARTESIAN_POINT('Ctrl Pts',(6.01980650390735,54.5064230730006,-0.581902777788305));
#6490=CARTESIAN_POINT('Ctrl Pts',(5.97393171253709,54.4893248150252,0.971080814223057));
#6491=CARTESIAN_POINT('Ctrl Pts',(5.7930658586323,54.4797353869317,1.75249128737854));
#6492=CARTESIAN_POINT('Ctrl Pts',(5.14386777267488,54.4601651694279,3.18549585271706));
#6493=CARTESIAN_POINT('Ctrl Pts',(4.68730851567618,54.4503813677914,3.82569012415617));
#6494=CARTESIAN_POINT('Ctrl Pts',(3.567531469532,54.4319267117499,4.8839546464704));
#6495=CARTESIAN_POINT('Ctrl Pts',(2.91928061049845,54.4239910076312,5.29698889009077));
#6496=CARTESIAN_POINT('Ctrl Pts',(1.46664814592476,54.405833101824,5.87284350350165));
#6497=CARTESIAN_POINT('Ctrl Pts',(0.670565922328707,54.3958820740291,6.01595179329487));
#6498=CARTESIAN_POINT('Ctrl Pts',(-0.899932770857932,54.3762508403642,5.98189549108154));
#6499=CARTESIAN_POINT('Ctrl Pts',(-1.65942748180796,54.3667571564773,5.81715281562034));
#6500=CARTESIAN_POINT('Ctrl Pts',(-3.08289154815884,54.348963855648,5.20602692283899));
#6501=CARTESIAN_POINT('Ctrl Pts',(-3.73209849904746,54.3407265244756,4.76218271375655));
#6502=CARTESIAN_POINT('Ctrl Pts',(-4.83280106975809,54.321728751943,3.64273458553758));
#6503=CARTESIAN_POINT('Ctrl Pts',(-5.27035822490241,54.3117622631446,2.97469352834565));
#6504=CARTESIAN_POINT('Ctrl Pts',(-5.85013328313548,54.2925513733541,1.53480083158262));
#6505=CARTESIAN_POINT('Ctrl Pts',(-5.99750082653629,54.2834682218936,0.780817931910112));
#6506=CARTESIAN_POINT('Ctrl Pts',(-6.002542372019,54.2665977363468,-0.774700029943063));
#6507=CARTESIAN_POINT('Ctrl Pts',(-5.84742264239086,54.2571423451884,-1.56152891151443));
#6508=CARTESIAN_POINT('Ctrl Pts',(-5.2446726922113,54.237616080659,-3.01729011869803));
#6509=CARTESIAN_POINT('Ctrl Pts',(-4.80754953397616,54.2277752224983,-3.67397648292641));
#6510=CARTESIAN_POINT('Ctrl Pts',(-3.72147580711357,54.2091510136092,-4.76736224684963));
#6511=CARTESIAN_POINT('Ctrl Pts',(-3.08858384949118,54.2011072981186,-5.19978535068864));
#6512=CARTESIAN_POINT('Ctrl Pts',(-1.66322673748714,54.1832903342185,-5.81935749367896));
#6513=CARTESIAN_POINT('Ctrl Pts',(-0.878877032028892,54.1734859629003,-5.98822219076233));
#6514=CARTESIAN_POINT('Ctrl Pts',(-0.0562965174381724,54.1632037064679,
-5.99980198137835));
#6515=CARTESIAN_POINT('Ctrl Pts',(-0.0281438351033594,54.1628517979388,
-6.));
#6516=CARTESIAN_POINT('Ctrl Pts',(3.00272269393625E-14,54.1625,-6.));
#6517=CARTESIAN_POINT('Ctrl Pts',(3.12250225675825E-14,54.106249998771,
-6.));
#6518=CARTESIAN_POINT('Ctrl Pts',(-0.665995216701814,54.1145749389797,-6.));
#6519=CARTESIAN_POINT('Ctrl Pts',(-1.32831154621538,54.1228538930987,-5.88910260237697));
#6520=CARTESIAN_POINT('Ctrl Pts',(-2.68380168378572,54.1397975198183,-5.42074527927475));
#6521=CARTESIAN_POINT('Ctrl Pts',(-3.35350325734009,54.1477146049907,-5.03401298858342));
#6522=CARTESIAN_POINT('Ctrl Pts',(-4.5181561134759,54.165933691407,-4.02341851709745));
#6523=CARTESIAN_POINT('Ctrl Pts',(-4.99990180303044,54.1756255441917,-3.40625951036384));
#6524=CARTESIAN_POINT('Ctrl Pts',(-5.71022474619925,54.1952223283079,-2.00609127926203));
#6525=CARTESIAN_POINT('Ctrl Pts',(-5.92538144060666,54.2049331533687,-1.2332644606244));
#6526=CARTESIAN_POINT('Ctrl Pts',(-6.03952951974,54.2224130621164,0.315556918500252));
#6527=CARTESIAN_POINT('Ctrl Pts',(-5.95130265594012,54.2307010359501,1.07587410048442));
#6528=CARTESIAN_POINT('Ctrl Pts',(-5.48845800853437,54.2495301726062,2.54801175744083));
#6529=CARTESIAN_POINT('Ctrl Pts',(-5.10861550067973,54.2594285450217,3.24308205985808));
#6530=CARTESIAN_POINT('Ctrl Pts',(-4.09445984153902,54.2789167229654,4.45779978214083));
#6531=CARTESIAN_POINT('Ctrl Pts',(-3.46606168236284,54.2879242277415,4.96215375070386));
#6532=CARTESIAN_POINT('Ctrl Pts',(-2.07840524998668,54.3052699331462,5.68021403610727));
#6533=CARTESIAN_POINT('Ctrl Pts',(-1.33839842906827,54.3145200184076,5.89858218723038));
#6534=CARTESIAN_POINT('Ctrl Pts',(0.213479934968243,54.3339184979581,6.04861227994175));
#6535=CARTESIAN_POINT('Ctrl Pts',(1.01169570619217,54.3438961950984,5.96722408995027));
#6536=CARTESIAN_POINT('Ctrl Pts',(2.50744136059901,54.3625930157785,5.50518764661662));
#6537=CARTESIAN_POINT('Ctrl Pts',(3.19332323280763,54.3705899008775,5.13780476697635));
#6538=CARTESIAN_POINT('Ctrl Pts',(4.39027354821862,54.3886326673574,4.16214498033042));
#6539=CARTESIAN_POINT('Ctrl Pts',(4.88958746882181,54.3982470520664,3.56228519082363));
#6540=CARTESIAN_POINT('Ctrl Pts',(5.64320947287391,54.4178391026293,2.1875529510982));
#6541=CARTESIAN_POINT('Ctrl Pts',(5.88297354086154,54.4276259148414,1.42191381386779));
#6542=CARTESIAN_POINT('Ctrl Pts',(6.04660168590296,54.4453757161804,-0.123271845530199));
#6543=CARTESIAN_POINT('Ctrl Pts',(5.98249839701545,54.4534586343659,-0.88674078467215));
#6544=CARTESIAN_POINT('Ctrl Pts',(5.56684849579367,54.4721244012078,-2.37103488404048));
#6545=CARTESIAN_POINT('Ctrl Pts',(5.21074344315951,54.4819779770023,-3.07567187803633));
#6546=CARTESIAN_POINT('Ctrl Pts',(4.2407625315026,54.5014910036302,-4.31818932579503));
#6547=CARTESIAN_POINT('Ctrl Pts',(3.63254647488505,54.5108431678349,-4.8410110561471));
#6548=CARTESIAN_POINT('Ctrl Pts',(2.2759967354326,54.5278000395781,-5.6036122334027));
#6549=CARTESIAN_POINT('Ctrl Pts',(1.54668082782739,54.5369164884232,-5.84708390728187));
#6550=CARTESIAN_POINT('Ctrl Pts',(0.528449925791234,54.5496443746986,-5.98256511642262));
#6551=CARTESIAN_POINT('Ctrl Pts',(0.264086110120325,54.5529489223944,-6.));
#6552=CARTESIAN_POINT('Ctrl Pts',(2.41473507855972E-14,54.556249998771,
-6.));
#6553=CARTESIAN_POINT('Origin',(0.,50.,0.));
#6554=CARTESIAN_POINT('',(-8.83284460251102E-15,55.0625,-6.));
#6555=CARTESIAN_POINT('',(1.52537908614269E-14,55.006249998771,-6.));
#6556=CARTESIAN_POINT('',(-7.34788079488412E-16,50.,-6.));
#6557=CARTESIAN_POINT('Ctrl Pts',(-3.46944695195361E-14,55.0625,-6.));
#6558=CARTESIAN_POINT('Ctrl Pts',(0.243170996938084,55.0594603625383,-6.));
#6559=CARTESIAN_POINT('Ctrl Pts',(0.486616495026908,55.0564172938121,-5.98521738970615));
#6560=CARTESIAN_POINT('Ctrl Pts',(1.48607170177765,55.0439241037278,-5.86287970427564));
#6561=CARTESIAN_POINT('Ctrl Pts',(2.21859564233351,55.0347675544708,-5.62668817545351));
#6562=CARTESIAN_POINT('Ctrl Pts',(3.583522346217,55.0177059706723,-4.87742638094908));
#6563=CARTESIAN_POINT('Ctrl Pts',(4.19704545643206,55.0084745072065,-4.36070730516347));
#6564=CARTESIAN_POINT('Ctrl Pts',(5.18000952607178,54.9889794757186,-3.12734800698956));
#6565=CARTESIAN_POINT('Ctrl Pts',(5.54341604297027,54.9791111174456,-2.42556096848081));
#6566=CARTESIAN_POINT('Ctrl Pts',(5.9735386696846,54.9603947304027,-0.944946607204173));
#6567=CARTESIAN_POINT('Ctrl Pts',(6.04506231156067,54.9522570672934,-0.182482207805695));
#6568=CARTESIAN_POINT('Ctrl Pts',(5.89669431020368,54.9345898771,1.36388260891157));
#6569=CARTESIAN_POINT('Ctrl Pts',(5.66449374094429,54.9248254128607,2.13182411687757));
#6570=CARTESIAN_POINT('Ctrl Pts',(4.92412965534831,54.9052297552454,3.51454402462014));
#6571=CARTESIAN_POINT('Ctrl Pts',(4.4301701829403,54.8955905211087,4.11979069803384));
#6572=CARTESIAN_POINT('Ctrl Pts',(3.24316152613063,54.8774928793281,5.10625946708773));
#6573=CARTESIAN_POINT('Ctrl Pts',(2.56232823027645,54.8695291028784,5.47964030494605));
#6574=CARTESIAN_POINT('Ctrl Pts',(1.07208496965756,54.8509010621207,5.9567802161547));
#6575=CARTESIAN_POINT('Ctrl Pts',(0.273888437522632,54.840923605469,6.04628594794717));
#6576=CARTESIAN_POINT('Ctrl Pts',(-1.28092368736922,54.8214884539079,5.91142217391699));
#6577=CARTESIAN_POINT('Ctrl Pts',(-2.02371620559728,54.81220354743,5.70002346906044));
#6578=CARTESIAN_POINT('Ctrl Pts',(-3.41623463724428,54.7947970670344,4.99613549809339));
#6579=CARTESIAN_POINT('Ctrl Pts',(-4.04744457912879,54.7859176942241,4.50002714754593));
#6580=CARTESIAN_POINT('Ctrl Pts',(-5.07348642469305,54.7664922480945,3.29796683495025));
#6581=CARTESIAN_POINT('Ctrl Pts',(-5.46116494334903,54.7565811802079,2.60624789808891));
#6582=CARTESIAN_POINT('Ctrl Pts',(-5.93968782386747,54.7376988813085,1.13825115557217));
#6583=CARTESIAN_POINT('Ctrl Pts',(-6.03588614738751,54.7293260283239,0.378902501922215));
#6584=CARTESIAN_POINT('Ctrl Pts',(-5.93799646795637,54.7119360578891,-1.17099752318919));
#6585=CARTESIAN_POINT('Ctrl Pts',(-5.73097417840607,54.7022524150224,-1.94600975911659));
#6586=CARTESIAN_POINT('Ctrl Pts',(-5.03506882783893,54.6826584748905,-3.35423927518282));
#6587=CARTESIAN_POINT('Ctrl Pts',(-4.55922402286184,54.6729431409721,-3.97697425342747));
#6588=CARTESIAN_POINT('Ctrl Pts',(-3.40522375135924,54.6546671349834,-4.99897700239477));
#6589=CARTESIAN_POINT('Ctrl Pts',(-2.74072116488649,54.6467590145611,-5.39200952355117));
#6590=CARTESIAN_POINT('Ctrl Pts',(-1.37124203932091,54.6296405254915,-5.88174277618126));
#6591=CARTESIAN_POINT('Ctrl Pts',(-0.687741080113753,54.6210967635014,-5.99999999999999));
#6592=CARTESIAN_POINT('Ctrl Pts',(-2.33146835171283E-14,54.6125,-6.));
#6593=CARTESIAN_POINT('Ctrl Pts',(2.4980018054066E-14,54.556249998771,-6.));
#6594=CARTESIAN_POINT('Ctrl Pts',(-0.524082563586572,54.5628010308158,-6.));
#6595=CARTESIAN_POINT('Ctrl Pts',(-1.04707144064502,54.5693383917791,-5.93133051383516));
#6596=CARTESIAN_POINT('Ctrl Pts',(-2.30620672576332,54.585077582843,-5.59336178117351));
#6597=CARTESIAN_POINT('Ctrl Pts',(-3.01071206136714,54.593257344516,-5.247846484898));
#6598=CARTESIAN_POINT('Ctrl Pts',(-4.24333742521803,54.6110988001506,-4.31137999639267));
#6599=CARTESIAN_POINT('Ctrl Pts',(-4.76145033958675,54.6206167190358,-3.73128494208711));
#6600=CARTESIAN_POINT('Ctrl Pts',(-5.56565134150618,54.6402674130825,-2.38033724741197));
#6601=CARTESIAN_POINT('Ctrl Pts',(-5.83351432249087,54.6502119037212,-1.61635531603474));
#6602=CARTESIAN_POINT('Ctrl Pts',(-6.04769396257433,54.6683072317106,-0.0684371911720527));
#6603=CARTESIAN_POINT('Ctrl Pts',(-6.00761182676598,54.6762638149825,0.69849130020703));
#6604=CARTESIAN_POINT('Ctrl Pts',(-5.63849769195529,54.6947638196598,2.19434038398171));
#6605=CARTESIAN_POINT('Ctrl Pts',(-5.30598207159103,54.7045636698139,2.90763378097386));
#6606=CARTESIAN_POINT('Ctrl Pts',(-4.37812463732207,54.7241241274613,4.17885271964518));
#6607=CARTESIAN_POINT('Ctrl Pts',(-3.7871338804005,54.7336874036299,4.72106165828979));
#6608=CARTESIAN_POINT('Ctrl Pts',(-2.45780508178541,54.7507092371596,5.52598294584271));
#6609=CARTESIAN_POINT('Ctrl Pts',(-1.73898164930581,54.7595127281547,5.7925185962507));
#6610=CARTESIAN_POINT('Ctrl Pts',(-0.211522394103572,54.7786059688447,6.04793647814097));
#6611=CARTESIAN_POINT('Ctrl Pts',(0.584595403767378,54.7885574413181,6.02333195023259));
#6612=CARTESIAN_POINT('Ctrl Pts',(2.11735082107309,54.8077168840344,5.66852444778916));
#6613=CARTESIAN_POINT('Ctrl Pts',(2.83951320933961,54.8161523731448,5.34345370764666));
#6614=CARTESIAN_POINT('Ctrl Pts',(4.10462434844559,54.8338045050574,4.4432318665157));
#6615=CARTESIAN_POINT('Ctrl Pts',(4.6392550826848,54.8432247738107,3.88169391275978));
#6616=CARTESIAN_POINT('Ctrl Pts',(5.48405859603673,54.8627923630686,2.56186498053673));
#6617=CARTESIAN_POINT('Ctrl Pts',(5.77603544192931,54.8727582598742,1.80982777855984));
#6618=CARTESIAN_POINT('Ctrl Pts',(6.04243628777694,54.8910943519024,0.269818751685842));
#6619=CARTESIAN_POINT('Ctrl Pts',(6.02766608938643,54.8990014361889,-0.501080033249619));
#6620=CARTESIAN_POINT('Ctrl Pts',(5.70698531737599,54.9173242780495,-2.00852653209502));
#6621=CARTESIAN_POINT('Ctrl Pts',(5.39916244932141,54.9270583443147,-2.72999944092045));
#6622=CARTESIAN_POINT('Ctrl Pts',(4.51584446455605,54.9466482719774,-4.02965556615108));
#6623=CARTESIAN_POINT('Ctrl Pts',(3.9432806003685,54.9563085395483,-4.59146295824019));
#6624=CARTESIAN_POINT('Ctrl Pts',(2.64248979487433,54.9736234368491,-5.4399327353421));
#6625=CARTESIAN_POINT('Ctrl Pts',(1.93413273845439,54.9820733395403,-5.7301633782239));
#6626=CARTESIAN_POINT('Ctrl Pts',(0.797703277241862,54.9962787078055,-5.96022548855814));
#6627=CARTESIAN_POINT('Ctrl Pts',(0.398870320543266,55.0012641197642,-6.));
#6628=CARTESIAN_POINT('Ctrl Pts',(3.81639164714898E-14,55.006249998771,
-6.));
#6629=CARTESIAN_POINT('Origin',(0.,50.,0.));
#6630=CARTESIAN_POINT('',(-6.36086364924407E-15,55.5125,-6.));
#6631=CARTESIAN_POINT('',(8.65316803533519E-15,55.456249998771,-6.));
#6632=CARTESIAN_POINT('',(-7.34788079488412E-16,50.,-6.));
#6633=CARTESIAN_POINT('Ctrl Pts',(-3.46250805804971E-14,55.5125,-6.));
#6634=CARTESIAN_POINT('Ctrl Pts',(0.376703946330025,55.5077912006709,-6.));
#6635=CARTESIAN_POINT('Ctrl Pts',(0.753472588888227,55.5030815926389,-5.96452369981927));
#6636=CARTESIAN_POINT('Ctrl Pts',(1.87073150335176,55.4891158562081,-5.75120440797882));
#6637=CARTESIAN_POINT('Ctrl Pts',(2.5824631340013,55.4805601853587,-5.46871532290478));
#6638=CARTESIAN_POINT('Ctrl Pts',(3.89264334169019,55.4633405323271,-4.6344648083913));
#6639=CARTESIAN_POINT('Ctrl Pts',(4.47131370817137,55.4537107987603,-4.07900361752885));
#6640=CARTESIAN_POINT('Ctrl Pts',(5.36930891312379,55.4341280670817,-2.78848612586233));
#6641=CARTESIAN_POINT('Ctrl Pts',(5.68523510906606,55.4243713528467,-2.06959954574193));
#6642=CARTESIAN_POINT('Ctrl Pts',(6.02178549004339,55.4059899565657,-0.565906344247707));
#6643=CARTESIAN_POINT('Ctrl Pts',(6.04488833118811,55.3980759709811,0.203650477614851));
#6644=CARTESIAN_POINT('Ctrl Pts',(5.79567389144728,55.3798183574028,1.74633255200975));
#6645=CARTESIAN_POINT('Ctrl Pts',(5.51158572968284,55.369858312968,2.50238366903789));
#6646=CARTESIAN_POINT('Ctrl Pts',(4.68002966528737,55.3502611620082,3.83259181253258));
#6647=CARTESIAN_POINT('Ctrl Pts',(4.15076842647487,55.3408077395651,4.40029245259052));
#6648=CARTESIAN_POINT('Ctrl Pts',(2.89634695185098,55.3230926721373,5.31249970824152));
#6649=CARTESIAN_POINT('Ctrl Pts',(2.18006863674793,55.3147508579593,5.64435900304111));
#6650=CARTESIAN_POINT('Ctrl Pts',(0.65301674366652,55.2956627092958,6.01641659700119));
#6651=CARTESIAN_POINT('Ctrl Pts',(-0.143697171846589,55.2857037853519,6.05004525969472));
#6652=CARTESIAN_POINT('Ctrl Pts',(-1.67538998151804,55.266557625231,5.81131134918754));
#6653=CARTESIAN_POINT('Ctrl Pts',(-2.39767714231781,55.2576212337002,5.55242057122521));
#6654=CARTESIAN_POINT('Ctrl Pts',(-3.73608308927647,55.2406948435203,4.76155665670778));
#6655=CARTESIAN_POINT('Ctrl Pts',(-4.33284626103593,55.2311650493507,4.22577335789718));
#6656=CARTESIAN_POINT('Ctrl Pts',(-5.27481565079531,55.2116187796453,2.96401258647136));
#6657=CARTESIAN_POINT('Ctrl Pts',(-5.61522017998204,55.2017999578695,2.25352132977259));
#6658=CARTESIAN_POINT('Ctrl Pts',(-5.99986293011047,55.1832441412076,0.761482005930106));
#6659=CARTESIAN_POINT('Ctrl Pts',(-6.04799029994773,55.1752538979774,-0.00425312209671055));
#6660=CARTESIAN_POINT('Ctrl Pts',(-5.85040814233194,55.1572365006543,-1.55455488134153));
#6661=CARTESIAN_POINT('Ctrl Pts',(-5.59029581047135,55.147301071778,-2.32217456232466));
#6662=CARTESIAN_POINT('Ctrl Pts',(-4.79921218024328,55.1276281671419,-3.68274730144777));
#6663=CARTESIAN_POINT('Ctrl Pts',(-4.28647314765261,55.1180811516861,-4.26863279389512));
#6664=CARTESIAN_POINT('Ctrl Pts',(-3.06417633838736,55.1001807055688,-5.21651178354219));
#6665=CARTESIAN_POINT('Ctrl Pts',(-2.36514495870567,55.0920643119838,-5.56841679012325));
#6666=CARTESIAN_POINT('Ctrl Pts',(-1.09060147835293,55.0761325184794,-5.92546814491037));
#6667=CARTESIAN_POINT('Ctrl Pts',(-0.545992672507869,55.0693249084063,-5.99999999999999));
#6668=CARTESIAN_POINT('Ctrl Pts',(-2.55351295663786E-14,55.0625,-6.));
#6669=CARTESIAN_POINT('Ctrl Pts',(2.67147415300428E-14,55.006249998771,
-6.));
#6670=CARTESIAN_POINT('Ctrl Pts',(-0.383498096873053,55.0110437249819,-6.));
#6671=CARTESIAN_POINT('Ctrl Pts',(-0.767030733126266,55.0158378829351,-5.96323238459905));
#6672=CARTESIAN_POINT('Ctrl Pts',(-1.92341860149788,55.0302927312897,-5.73836805133425));
#6673=CARTESIAN_POINT('Ctrl Pts',(-2.66390770238158,55.0390710339514,-5.43433369990439));
#6674=CARTESIAN_POINT('Ctrl Pts',(-3.96150517296733,55.05652800478,-4.57089605970513));
#6675=CARTESIAN_POINT('Ctrl Pts',(-4.51204186370488,55.0658414586601,-4.02840854953488));
#6676=CARTESIAN_POINT('Ctrl Pts',(-5.39638537330542,55.0853059424018,-2.74093252440032));
#6677=CARTESIAN_POINT('Ctrl Pts',(-5.71203585602825,55.0952824329659,-2.0015846935231));
#6678=CARTESIAN_POINT('Ctrl Pts',(-6.03067862274505,55.1138523039486,-0.470141978956567));
#6679=CARTESIAN_POINT('Ctrl Pts',(-6.04128052820748,55.1217941051577,0.305035826766368));
#6680=CARTESIAN_POINT('Ctrl Pts',(-5.76842964141191,55.1399375910254,1.82352872578303));
#6681=CARTESIAN_POINT('Ctrl Pts',(-5.48507891182408,55.1495970803031,2.55224150333299));
#6682=CARTESIAN_POINT('Ctrl Pts',(-4.64644024297387,55.1691942904959,3.87836597494945));
#6683=CARTESIAN_POINT('Ctrl Pts',(-4.09266447021715,55.1789391921554,4.45883883889243));
#6684=CARTESIAN_POINT('Ctrl Pts',(-2.82041073021032,55.1965364144534,5.34986456454548));
#6685=CARTESIAN_POINT('Ctrl Pts',(-2.12191903657733,55.2047260108138,5.66332403510793));
#6686=CARTESIAN_POINT('Ctrl Pts',(-0.621212253847653,55.2234848455979,6.01896338011437));
#6687=CARTESIAN_POINT('Ctrl Pts',(0.169198820019541,55.2333649840212,6.04856958122179));
#6688=CARTESIAN_POINT('Ctrl Pts',(1.73468835005995,55.2529336031467,5.79944910313727));
#6689=CARTESIAN_POINT('Ctrl Pts',(2.4932084072145,55.2621197300586,5.51603414832992));
#6690=CARTESIAN_POINT('Ctrl Pts',(3.82167666488108,55.2793856676905,4.68806665616739));
#6691=CARTESIAN_POINT('Ctrl Pts',(4.38673093219715,55.2885893283747,4.16410313374755));
#6692=CARTESIAN_POINT('Ctrl Pts',(5.30758874303518,55.3079374972146,2.90845336063413));
#6693=CARTESIAN_POINT('Ctrl Pts',(5.64528357279742,55.3179140263612,2.18182927535854));
#6694=CARTESIAN_POINT('Ctrl Pts',(6.01358028789105,55.3366990892299,0.659175706319895));
#6695=CARTESIAN_POINT('Ctrl Pts',(6.04840302459413,55.3447500396245,-0.120325316236857));
#6696=CARTESIAN_POINT('Ctrl Pts',(5.82046622292647,55.3627212936052,-1.64883927418895));
#6697=CARTESIAN_POINT('Ctrl Pts',(5.56012447741785,55.3723023405631,-2.38359010377172));
#6698=CARTESIAN_POINT('Ctrl Pts',(4.76396909667191,55.3918869071758,-3.73307434931714));
#6699=CARTESIAN_POINT('Ctrl Pts',(4.22832460066992,55.4017011341472,-4.3304193087725));
#6700=CARTESIAN_POINT('Ctrl Pts',(2.98320792615936,55.4195567595843,-5.26098288599923));
#6701=CARTESIAN_POINT('Ctrl Pts',(2.29359292232722,55.4275800872419,-5.59615121010581));
#6702=CARTESIAN_POINT('Ctrl Pts',(1.05013028978537,55.4431233701486,-5.93092063589006));
#6703=CARTESIAN_POINT('Ctrl Pts',(0.52564419070393,55.4496794463872,-6.));
#6704=CARTESIAN_POINT('Ctrl Pts',(3.92741394961149E-14,55.456249998771,
-6.));
#6705=CARTESIAN_POINT('Origin',(0.,50.,0.));
#6706=CARTESIAN_POINT('',(4.30578759205125E-16,55.9625,-6.));
#6707=CARTESIAN_POINT('',(-6.33484279710442E-15,55.906249998771,-6.));
#6708=CARTESIAN_POINT('',(-7.34788079488412E-16,50.,-6.));
#6709=CARTESIAN_POINT('Ctrl Pts',(-2.31759056390501E-14,55.9625,-6.));
#6710=CARTESIAN_POINT('Ctrl Pts',(0.506510355492559,55.9561686205563,-6.));
#6711=CARTESIAN_POINT('Ctrl Pts',(1.01209912649085,55.9498487609188,-5.93585868886586));
#6712=CARTESIAN_POINT('Ctrl Pts',(2.23972937663833,55.934503382792,-5.61786356684971));
#6713=CARTESIAN_POINT('Ctrl Pts',(2.93211714923827,55.9264354497199,-5.28956140569632));
#6714=CARTESIAN_POINT('Ctrl Pts',(4.18586379090878,55.9086609288615,-4.37147246239368));
#6715=CARTESIAN_POINT('Ctrl Pts',(4.72729822672339,55.8988675897434,-3.77939986348097));
#6716=CARTESIAN_POINT('Ctrl Pts',(5.53695585424453,55.8792769970504,-2.43715447829796));
#6717=CARTESIAN_POINT('Ctrl Pts',(5.80458380678377,55.8696702471273,-1.70423600408193));
#6718=CARTESIAN_POINT('Ctrl Pts',(6.04674334504191,55.8516440612997,-0.178859160276753));
#6719=CARTESIAN_POINT('Ctrl Pts',(6.01963510658597,55.8436357324319,0.599242189053428));
#6720=CARTESIAN_POINT('Ctrl Pts',(5.66712365275588,55.8249183119528,2.1247608466305));
#6721=CARTESIAN_POINT('Ctrl Pts',(5.33638643972422,55.814940737021,2.85549851929398));
#6722=CARTESIAN_POINT('Ctrl Pts',(4.42702037453283,55.7955536697512,4.12137633788628));
#6723=CARTESIAN_POINT('Ctrl Pts',(3.86651644869223,55.7863142436256,4.65127087115331));
#6724=CARTESIAN_POINT('Ctrl Pts',(2.54786180622585,55.7689869752017,5.49056975257084));
#6725=CARTESIAN_POINT('Ctrl Pts',(1.79513813675954,55.7599392267095,5.78061097099999));
#6726=CARTESIAN_POINT('Ctrl Pts',(0.23458113017717,55.7404322641272,6.04649552222604));
#6727=CARTESIAN_POINT('Ctrl Pts',(-0.556964089759994,55.730537948878,6.02535719121178));
#6728=CARTESIAN_POINT('Ctrl Pts',(-2.06199924228826,55.7117250094714,5.68539383393839));
#6729=CARTESIAN_POINT('Ctrl Pts',(-2.76361918902967,55.7034610872385,5.37939944167112));
#6730=CARTESIAN_POINT('Ctrl Pts',(-4.04510199417962,55.685953988623,4.50202738844765));
#6731=CARTESIAN_POINT('Ctrl Pts',(-4.60498874435356,55.6762351251842,3.927488006763));
#6732=CARTESIAN_POINT('Ctrl Pts',(-5.45808318515566,55.6566379085014,2.60970897944998));
#6733=CARTESIAN_POINT('Ctrl Pts',(-5.74932024339951,55.6469533803752,1.88323638612024));
#6734=CARTESIAN_POINT('Ctrl Pts',(-6.03757286035596,55.628751677179,0.36825779370989));
#6735=CARTESIAN_POINT('Ctrl Pts',(-6.03518566331545,55.620830193446,-0.405504682015357));
#6736=CARTESIAN_POINT('Ctrl Pts',(-5.7334376873049,55.6023351233639,-1.93979179733037));
#6737=CARTESIAN_POINT('Ctrl Pts',(-5.42539117238217,55.5923608738131,-2.68332276511667));
#6738=CARTESIAN_POINT('Ctrl Pts',(-4.55371198609171,55.5728608728174,-3.98139148411494));
#6739=CARTESIAN_POINT('Ctrl Pts',(-4.00824961913072,55.5635118891683,-4.53009075594725));
#6740=CARTESIAN_POINT('Ctrl Pts',(-2.72115707341145,55.545991162172,-5.40548295984068));
#6741=CARTESIAN_POINT('Ctrl Pts',(-1.98666726293254,55.5373333407866,-5.71638974522215));
#6742=CARTESIAN_POINT('Ctrl Pts',(-0.813017784230776,55.5226627223029,-5.95867972578508));
#6743=CARTESIAN_POINT('Ctrl Pts',(-0.406546568500345,55.5175818321062,-6.));
#6744=CARTESIAN_POINT('Ctrl Pts',(-2.43555176027144E-14,55.5125,-6.));
#6745=CARTESIAN_POINT('Ctrl Pts',(3.10862446895044E-14,55.456249998771,
-6.));
#6746=CARTESIAN_POINT('Ctrl Pts',(-0.252210903516962,55.4594026350649,-6.));
#6747=CARTESIAN_POINT('Ctrl Pts',(-0.504688423457114,55.4625586040642,-5.98409784058804));
#6748=CARTESIAN_POINT('Ctrl Pts',(-1.54373724533781,55.4755467143377,-5.85213938017255));
#6749=CARTESIAN_POINT('Ctrl Pts',(-2.30391117524793,55.4850488884616,-5.59666644130015));
#6750=CARTESIAN_POINT('Ctrl Pts',(-3.65187175733235,55.5018983957376,-4.82109477946861));
#6751=CARTESIAN_POINT('Ctrl Pts',(-4.23331191747355,55.5109480403995,-4.31951835605545));
#6752=CARTESIAN_POINT('Ctrl Pts',(-5.1959362139153,55.5301362886266,-3.10275530806472));
#6753=CARTESIAN_POINT('Ctrl Pts',(-5.55907359665902,55.5401003115312,-2.39197576474886));
#6754=CARTESIAN_POINT('Ctrl Pts',(-5.98607499914932,55.5591303586157,-0.880584690310904));
#6755=CARTESIAN_POINT('Ctrl Pts',(-6.04974036764568,55.5674032084568,-0.0956935454188609));
#6756=CARTESIAN_POINT('Ctrl Pts',(-5.87426437626053,55.5851687624621,1.44410692567844));
#6757=CARTESIAN_POINT('Ctrl Pts',(-5.64076913631869,55.594648290711,2.18497969585381));
#6758=CARTESIAN_POINT('Ctrl Pts',(-4.89196010651508,55.6142677812028,3.56502549961348));
#6759=CARTESIAN_POINT('Ctrl Pts',(-4.37327273364698,55.6242222315692,4.18511394105391));
#6760=CARTESIAN_POINT('Ctrl Pts',(-3.1530932458043,55.6424157760385,5.16129063278652));
#6761=CARTESIAN_POINT('Ctrl Pts',(-2.47263399832919,55.6503420737918,5.51969218998909));
#6762=CARTESIAN_POINT('Ctrl Pts',(-0.998344881824021,55.6687706877482,5.96736898710037));
#6763=CARTESIAN_POINT('Ctrl Pts',(-0.216398092781286,55.6785450226112,6.04643284268571));
#6764=CARTESIAN_POINT('Ctrl Pts',(1.34961157525821,55.6981201434617,5.8999504421065));
#6765=CARTESIAN_POINT('Ctrl Pts',(2.11793378939434,55.7077241711384,5.66967751177729));
#6766=CARTESIAN_POINT('Ctrl Pts',(3.4892697862692,55.7248658710993,4.93977576174127));
#6767=CARTESIAN_POINT('Ctrl Pts',(4.08570796533894,55.7335147004569,4.45908148989135));
#6768=CARTESIAN_POINT('Ctrl Pts',(5.08605410587349,55.752540440314,3.27910903892516));
#6769=CARTESIAN_POINT('Ctrl Pts',(5.47216468472763,55.7624807928114,2.58377965513738));
#6770=CARTESIAN_POINT('Ctrl Pts',(5.95365105266994,55.7817284375683,1.08374467820946));
#6771=CARTESIAN_POINT('Ctrl Pts',(6.04435521787812,55.7902941311579,0.293630878490182));
#6772=CARTESIAN_POINT('Ctrl Pts',(5.9169993760804,55.807866799235,-1.25613373511938));
#6773=CARTESIAN_POINT('Ctrl Pts',(5.70804226618502,55.8172442820665,-2.00174704940243));
#6774=CARTESIAN_POINT('Ctrl Pts',(5.00701244719134,55.8367719223822,-3.4008934375671));
#6775=CARTESIAN_POINT('Ctrl Pts',(4.51104662686718,55.8467434818924,-4.03568064847992));
#6776=CARTESIAN_POINT('Ctrl Pts',(3.32426749193355,55.8651764922436,-5.05326195358436));
#6777=CARTESIAN_POINT('Ctrl Pts',(2.65297920336261,55.8730877587289,-5.43579915260006));
#6778=CARTESIAN_POINT('Ctrl Pts',(1.30624861040293,55.8899218911409,-5.89276769691465));
#6779=CARTESIAN_POINT('Ctrl Pts',(0.654900599338993,55.8980637412792,-6.));
#6780=CARTESIAN_POINT('Ctrl Pts',(-1.98452365651747E-14,55.906249998771,
-6.));
#6781=CARTESIAN_POINT('Origin',(0.,50.,0.));
#6782=CARTESIAN_POINT('',(-1.96575190926063E-14,56.4125,-6.));
#6783=CARTESIAN_POINT('',(-4.32256356497133E-15,56.3562499987709,-6.));
#6784=CARTESIAN_POINT('',(-7.34788079488412E-16,50.,-6.));
#6785=CARTESIAN_POINT('Ctrl Pts',(1.59594559789866E-14,56.4125,-6.));
#6786=CARTESIAN_POINT('Ctrl Pts',(0.655375591716446,56.4043078051035,-6.));
#6787=CARTESIAN_POINT('Ctrl Pts',(1.30732882068663,56.3961583897414,-5.89261098724614));
#6788=CARTESIAN_POINT('Ctrl Pts',(2.65590763722434,56.3793011545347,-5.43455999387956));
#6789=CARTESIAN_POINT('Ctrl Pts',(3.32816065133725,56.371376638691,-5.05090428275669));
#6790=CARTESIAN_POINT('Ctrl Pts',(4.49799175700267,56.3531854412059,-4.04587574413293));
#6791=CARTESIAN_POINT('Ctrl Pts',(4.98258729451814,56.3435053739532,-3.43145079870755));
#6792=CARTESIAN_POINT('Ctrl Pts',(5.69989537662752,56.3239079934447,-2.03526034708743));
#6793=CARTESIAN_POINT('Ctrl Pts',(5.91900359014787,56.3141843310689,-1.26352907871823));
#6794=CARTESIAN_POINT('Ctrl Pts',(6.04106600107415,56.2966608626863,0.284746825533261));
#6795=CARTESIAN_POINT('Ctrl Pts',(5.95671079979978,56.288411058258,1.04554755236564));
#6796=CARTESIAN_POINT('Ctrl Pts',(5.50016128983585,56.2695539572171,2.52390294774796));
#6797=CARTESIAN_POINT('Ctrl Pts',(5.1211965582148,56.2596049286264,3.22415944935899));
#6798=CARTESIAN_POINT('Ctrl Pts',(4.13262816737534,56.2405274921602,4.41570731546272));
#6799=CARTESIAN_POINT('Ctrl Pts',(3.54093488582301,56.2317616860728,4.90294124689549));
#6800=CARTESIAN_POINT('Ctrl Pts',(2.1769282763679,56.2147116034546,5.64728331917592));
#6801=CARTESIAN_POINT('Ctrl Pts',(1.41108733546057,56.2051385916932,5.88554479318212));
#6802=CARTESIAN_POINT('Ctrl Pts',(-0.154051268862532,56.1855743591392,6.04844370577617));
#6803=CARTESIAN_POINT('Ctrl Pts',(-0.937571873767269,56.1757803515779,5.97732115913926));
#6804=CARTESIAN_POINT('Ctrl Pts',(-2.41623675328628,56.1572970405839,5.5444969437559));
#6805=CARTESIAN_POINT('Ctrl Pts',(-3.09957176867773,56.1493488123132,5.19348606835151));
#6806=CARTESIAN_POINT('Ctrl Pts',(-4.32991740497706,56.1312303713413,4.23011656908343));
#6807=CARTESIAN_POINT('Ctrl Pts',(-4.8555092940329,56.1212833886199,3.61470428341965));
#6808=CARTESIAN_POINT('Ctrl Pts',(-5.61890970623177,56.101639711652,2.24084856725757));
#6809=CARTESIAN_POINT('Ctrl Pts',(-5.85993019338523,56.0921306525639,1.50159255851692));
#6810=CARTESIAN_POINT('Ctrl Pts',(-6.05012504695993,56.0743068999117,-0.0350861342543961));
#6811=CARTESIAN_POINT('Ctrl Pts',(-5.99461604293912,56.0661065790627,-0.818430606491861));
#6812=CARTESIAN_POINT('Ctrl Pts',(-5.58416036006447,56.0471445058752,-2.33309519696156));
#6813=CARTESIAN_POINT('Ctrl Pts',(-5.22812325350618,56.0371755875623,-3.04842630508126));
#6814=CARTESIAN_POINT('Ctrl Pts',(-4.27712108424128,56.0179400054575,-4.27627190765333));
#6815=CARTESIAN_POINT('Ctrl Pts',(-3.70021645348818,56.0088357393135,-4.78421194524034));
#6816=CARTESIAN_POINT('Ctrl Pts',(-2.35933157194477,55.9919105321677,-5.57353536219895));
#6817=CARTESIAN_POINT('Ctrl Pts',(-1.60167263802065,55.9825209079752,-5.83655998386992));
#6818=CARTESIAN_POINT('Ctrl Pts',(-0.544202575513397,55.9693025321939,-5.98150876757896));
#6819=CARTESIAN_POINT('Ctrl Pts',(-0.271968436546483,55.9658996054568,-6.));
#6820=CARTESIAN_POINT('Ctrl Pts',(-3.30985239216375E-14,55.9625,-6.));
#6821=CARTESIAN_POINT('Ctrl Pts',(-2.78943534937071E-14,55.906249998771,
-6.));
#6822=CARTESIAN_POINT('Ctrl Pts',(-0.119270180566787,55.907740876028,-6.));
#6823=CARTESIAN_POINT('Ctrl Pts',(-0.238658191670233,55.9092332261669,-5.99644370777172));
#6824=CARTESIAN_POINT('Ctrl Pts',(-1.15097298881717,55.9206371611312,-5.94191079972275));
#6825=CARTESIAN_POINT('Ctrl Pts',(-1.92669402478814,55.9303336740808,-5.73750039954501));
#6826=CARTESIAN_POINT('Ctrl Pts',(-3.32126851885456,55.9477658552566,-5.05417095172651));
#6827=CARTESIAN_POINT('Ctrl Pts',(-3.93304275666383,55.9560978579313,-4.59419853981487));
#6828=CARTESIAN_POINT('Ctrl Pts',(-4.97046981399306,55.9749552855053,-3.45118278885069));
#6829=CARTESIAN_POINT('Ctrl Pts',(-5.3788842150237,55.9848605335407,-2.77197333408993));
#6830=CARTESIAN_POINT('Ctrl Pts',(-5.91480788525159,56.0043155350143,-1.28421295529728));
#6831=CARTESIAN_POINT('Ctrl Pts',(-6.03284998524064,56.0132540892278,-0.488724428843167));
#6832=CARTESIAN_POINT('Ctrl Pts',(-5.95307864390457,56.0306320858508,1.07053013027671));
#6833=CARTESIAN_POINT('Ctrl Pts',(-5.76824859512135,56.0399007335379,1.82001944980712));
#6834=CARTESIAN_POINT('Ctrl Pts',(-5.11449349917068,56.0593188805931,3.2363453578896));
#6835=CARTESIAN_POINT('Ctrl Pts',(-4.64117525801476,56.0692965738505,3.88477476699456));
#6836=CARTESIAN_POINT('Ctrl Pts',(-3.49281748541018,56.0878739702295,4.93787646592986));
#6837=CARTESIAN_POINT('Ctrl Pts',(-2.837096009414,56.0957862986533,5.34165539099934));
#6838=CARTESIAN_POINT('Ctrl Pts',(-1.37551778539592,56.1140560264535,5.8946789976836));
#6839=CARTESIAN_POINT('Ctrl Pts',(-0.578636157799252,56.1240170467985,6.02531808526819));
#6840=CARTESIAN_POINT('Ctrl Pts',(0.988783613055412,56.1436097939341,5.96770974701454));
#6841=CARTESIAN_POINT('Ctrl Pts',(1.7446548179888,56.1530581839958,5.79201578404849));
#6842=CARTESIAN_POINT('Ctrl Pts',(3.16108939615775,56.1707636162229,5.15941578064434));
#6843=CARTESIAN_POINT('Ctrl Pts',(3.80617671912254,56.1791192213777,4.70373101437893));
#6844=CARTESIAN_POINT('Ctrl Pts',(4.89006630320523,56.1982183667389,3.56521148303067));
#6845=CARTESIAN_POINT('Ctrl Pts',(5.31630477201846,56.2081762283405,2.89143252553516));
#6846=CARTESIAN_POINT('Ctrl Pts',(5.87286095503918,56.2273143187955,1.44485931946931));
#6847=CARTESIAN_POINT('Ctrl Pts',(6.00851807636355,56.2362297678481,0.689771261951205));
#6848=CARTESIAN_POINT('Ctrl Pts',(5.99025571610193,56.2531707988027,-0.864630364559025));
#6849=CARTESIAN_POINT('Ctrl Pts',(5.82334149419617,56.2627057874727,-1.64906691766854));
#6850=CARTESIAN_POINT('Ctrl Pts',(5.19927143500941,56.2822543761502,-3.09458117064177));
#6851=CARTESIAN_POINT('Ctrl Pts',(4.75319161261995,56.2920703642246,-3.74379900224259));
#6852=CARTESIAN_POINT('Ctrl Pts',(3.65167466294551,56.3106176781953,-4.82116536902607));
#6853=CARTESIAN_POINT('Ctrl Pts',(3.01182230798196,56.3186022199212,-5.24473876155051));
#6854=CARTESIAN_POINT('Ctrl Pts',(1.5780185312142,56.3365247671308,-5.84284081098096));
#6855=CARTESIAN_POINT('Ctrl Pts',(0.792860950716405,56.346339236887,-6.));
#6856=CARTESIAN_POINT('Ctrl Pts',(-3.28903571045203E-14,56.3562499987709,
-6.));
#6857=CARTESIAN_POINT('Origin',(0.,50.,0.));
#6858=CARTESIAN_POINT('',(1.97553982815868E-14,56.8625,-6.));
#6859=CARTESIAN_POINT('',(1.82982305617662E-14,56.806249998771,-6.));
#6860=CARTESIAN_POINT('',(-7.34788079488412E-16,50.,-6.));
#6861=CARTESIAN_POINT('Ctrl Pts',(5.19029264012261E-14,56.8625,-6.));
#6862=CARTESIAN_POINT('Ctrl Pts',(0.79230170443347,56.8525962286946,-6.));
#6863=CARTESIAN_POINT('Ctrl Pts',(1.57692203908962,56.8427884745114,-5.84306232652071));
#6864=CARTESIAN_POINT('Ctrl Pts',(3.01039884018676,56.8248700144976,-5.24555843097968));
#6865=CARTESIAN_POINT('Ctrl Pts',(3.65038030404161,56.8168864084426,-4.8221481831563));
#6866=CARTESIAN_POINT('Ctrl Pts',(4.7521810297415,56.7983405201061,-3.74507734898934));
#6867=CARTESIAN_POINT('Ctrl Pts',(5.19842465106967,56.788525009161,-3.09599816206786));
#6868=CARTESIAN_POINT('Ctrl Pts',(5.82288616449566,56.7689760372507,-1.65067451377228));
#6869=CARTESIAN_POINT('Ctrl Pts',(5.9900170998114,56.7594401809463,-0.866282931574435));
#6870=CARTESIAN_POINT('Ctrl Pts',(6.00870781223811,56.7424966987589,0.688097820879049));
#6871=CARTESIAN_POINT('Ctrl Pts',(5.87326509905218,56.7335847363924,1.44320666884808));
#6872=CARTESIAN_POINT('Ctrl Pts',(5.31713429155998,56.7144479987091,2.88990050189163));
#6873=CARTESIAN_POINT('Ctrl Pts',(4.89110382406863,56.7044903178273,3.56378285482827));
#6874=CARTESIAN_POINT('Ctrl Pts',(3.80752381648088,56.6853893334694,4.70265099948569));
#6875=CARTESIAN_POINT('Ctrl Pts',(3.16251190645564,56.6770313988307,5.15855339423183));
#6876=CARTESIAN_POINT('Ctrl Pts',(1.74620643543745,56.6593275804429,5.79154551234025));
#6877=CARTESIAN_POINT('Ctrl Pts',(0.990402786055763,56.6498800348257,5.96743864857926));
#6878=CARTESIAN_POINT('Ctrl Pts',(-0.576957627503505,56.6302880296562,6.02547594392505));
#6879=CARTESIAN_POINT('Ctrl Pts',(-1.37385210404051,56.6203268486995,5.89506426277027));
#6880=CARTESIAN_POINT('Ctrl Pts',(-2.83559237052781,56.6020550953684,5.34245766139812));
#6881=CARTESIAN_POINT('Ctrl Pts',(-3.4914506638857,56.5941430230773,4.93884724332227));
#6882=CARTESIAN_POINT('Ctrl Pts',(-4.62742573681593,56.5757721178423,3.89767122424419));
#6883=CARTESIAN_POINT('Ctrl Pts',(-5.09317321362636,56.566019397227,3.26565291573955));
#6884=CARTESIAN_POINT('Ctrl Pts',(-5.76454703716699,56.54643519543,1.84415970479431));
#6885=CARTESIAN_POINT('Ctrl Pts',(-5.95779467092296,56.5367998826718,1.06565921181134));
#6886=CARTESIAN_POINT('Ctrl Pts',(-6.02824627631527,56.5195630499973,-0.485935932386859));
#6887=CARTESIAN_POINT('Ctrl Pts',(-5.91853504504944,56.5110271148658,-1.24372602530261));
#6888=CARTESIAN_POINT('Ctrl Pts',(-5.4133585673446,56.4920557629773,-2.70456066906765));
#6889=CARTESIAN_POINT('Ctrl Pts',(-5.01242265950065,56.4821256339637,-3.39038624019974));
#6890=CARTESIAN_POINT('Ctrl Pts',(-3.96637907523528,56.4628090686586,-4.570840563839));
#6891=CARTESIAN_POINT('Ctrl Pts',(-3.33041263228381,56.4541301579035,-5.05302690239553));
#6892=CARTESIAN_POINT('Ctrl Pts',(-1.92967253351213,56.4366209066689,-5.73270782100113));
#6893=CARTESIAN_POINT('Ctrl Pts',(-1.18226194780873,56.4272782743476,-5.9321004182363));
#6894=CARTESIAN_POINT('Ctrl Pts',(-0.278410879134601,56.4159801359892,-5.99516091994516));
#6895=CARTESIAN_POINT('Ctrl Pts',(-0.139128323189838,56.4142391040399,-6.));
#6896=CARTESIAN_POINT('Ctrl Pts',(-3.15719672627779E-15,56.4125,-6.));
#6897=CARTESIAN_POINT('Ctrl Pts',(-2.79634361094744E-14,56.356249998771,
-6.));
#6898=CARTESIAN_POINT('Ctrl Pts',(-0.00925431949252112,56.3563656777646,
-6.));
#6899=CARTESIAN_POINT('Ctrl Pts',(-0.0185096884686758,56.3564813698768,
-5.99997858939597));
#6900=CARTESIAN_POINT('Ctrl Pts',(-0.799046772047178,56.3662380834215,-5.996366480783));
#6901=CARTESIAN_POINT('Ctrl Pts',(-1.56245757872404,56.375780718505,-5.84411035638461));
#6902=CARTESIAN_POINT('Ctrl Pts',(-2.99377584853423,56.3936721968776,-5.25727495839769));
#6903=CARTESIAN_POINT('Ctrl Pts',(-3.64762391318448,56.4017977100718,-4.82664253757592));
#6904=CARTESIAN_POINT('Ctrl Pts',(-4.76701621692779,56.4206793476575,-3.7287130186124));
#6905=CARTESIAN_POINT('Ctrl Pts',(-5.21720131349499,56.4306526218535,-3.06733589861962));
#6906=CARTESIAN_POINT('Ctrl Pts',(-5.82300969662807,56.4499413548937,-1.63528269760468));
#6907=CARTESIAN_POINT('Ctrl Pts',(-5.98351994764647,56.4590918575462,-0.882666107090339));
#6908=CARTESIAN_POINT('Ctrl Pts',(-6.01470652529258,56.4761376036864,0.673946893518462));
#6909=CARTESIAN_POINT('Ctrl Pts',(-5.87276684295458,56.4853870058037,1.46340278074942));
#6910=CARTESIAN_POINT('Ctrl Pts',(-5.2939284322367,56.5048849006054,2.93034863848238));
#6911=CARTESIAN_POINT('Ctrl Pts',(-4.86693149478656,56.5147510685449,3.59521939622588));
#6912=CARTESIAN_POINT('Ctrl Pts',(-3.79815452074611,56.5334597809641,4.70639754678297));
#6913=CARTESIAN_POINT('Ctrl Pts',(-3.17290832994337,56.5415886446467,5.14866957910816));
#6914=CARTESIAN_POINT('Ctrl Pts',(-1.7585265333779,56.5592684171037,5.79126668266434));
#6915=CARTESIAN_POINT('Ctrl Pts',(-0.977092871982791,56.5690363378712,5.97297738342711));
#6916=CARTESIAN_POINT('Ctrl Pts',(0.590525770206689,56.5886315708985,6.02081222645328));
#6917=CARTESIAN_POINT('Ctrl Pts',(1.36136697655774,56.5982670859779,5.8945391065037));
#6918=CARTESIAN_POINT('Ctrl Pts',(2.80851390396222,56.6163564225705,5.35766563810351));
#6919=CARTESIAN_POINT('Ctrl Pts',(3.47188226102197,56.6243247365624,4.95362155480435));
#6920=CARTESIAN_POINT('Ctrl Pts',(4.62865756826947,56.64296324636,3.89973430600555));
#6921=CARTESIAN_POINT('Ctrl Pts',(5.10420827628955,56.6529408032822,3.25260640731597));
#6922=CARTESIAN_POINT('Ctrl Pts',(5.76260847138282,56.6723705134876,1.83789419040876));
#6923=CARTESIAN_POINT('Ctrl Pts',(5.94980260893631,56.6816501951599,1.08875050227638));
#6924=CARTESIAN_POINT('Ctrl Pts',(6.03425140366107,56.6990475013165,-0.46958726618876));
#6925=CARTESIAN_POINT('Ctrl Pts',(5.91892429640393,56.7079457666895,-1.26453978936345));
#6926=CARTESIAN_POINT('Ctrl Pts',(5.38837502284035,56.7273807618557,-2.75355497399551));
#6927=CARTESIAN_POINT('Ctrl Pts',(4.98213291703594,56.7372899804404,-3.43438538763148));
#6928=CARTESIAN_POINT('Ctrl Pts',(3.94834137551491,56.7561642773249,-4.58105842476809));
#6929=CARTESIAN_POINT('Ctrl Pts',(3.33809854614214,56.7645237669442,-5.04307208402363));
#6930=CARTESIAN_POINT('Ctrl Pts',(1.94581237222651,56.7819273441181,-5.73104345580422));
#6931=CARTESIAN_POINT('Ctrl Pts',(1.17078731673957,56.7916151573117,-5.93803703272594));
#6932=CARTESIAN_POINT('Ctrl Pts',(0.251991343217977,56.8031001069807,-5.99603536758937));
#6933=CARTESIAN_POINT('Ctrl Pts',(0.125931641266464,56.8046758532551,-6.));
#6934=CARTESIAN_POINT('Ctrl Pts',(1.76941794549634E-15,56.806249998771,
-6.));
#6935=CARTESIAN_POINT('Origin',(0.,50.,0.));
#6936=CARTESIAN_POINT('',(3.74495777365502E-14,57.3125,-6.));
#6937=CARTESIAN_POINT('',(-3.54435027239952E-14,57.256249998771,-6.));
#6938=CARTESIAN_POINT('',(-7.34788079488412E-16,50.,-6.));
#6939=CARTESIAN_POINT('Ctrl Pts',(1.02071129326475E-13,57.3125,-6.));
#6940=CARTESIAN_POINT('Ctrl Pts',(0.125400103295474,57.3109324987088,-6.));
#6941=CARTESIAN_POINT('Ctrl Pts',(0.250927449357367,57.309363406883,-5.99606876480776));
#6942=CARTESIAN_POINT('Ctrl Pts',(1.16920671278006,57.2978849160902,-5.93834856646838));
#6943=CARTESIAN_POINT('Ctrl Pts',(1.94428762714173,57.2881964046607,-5.73156102449072));
#6944=CARTESIAN_POINT('Ctrl Pts',(3.33675657998753,57.2707905427501,-5.04395995896572));
#6945=CARTESIAN_POINT('Ctrl Pts',(3.947121550112,57.2624332788191,-4.582109327563));
#6946=CARTESIAN_POINT('Ctrl Pts',(4.98120359387457,57.2435603269992,-3.43572826371665));
#6947=CARTESIAN_POINT('Ctrl Pts',(5.38761940453579,57.2336514214288,-2.75502705365286));
#6948=CARTESIAN_POINT('Ctrl Pts',(5.91859783697493,57.2142148248932,-1.26611171583379));
#6949=CARTESIAN_POINT('Ctrl Pts',(6.03414160801522,57.2053133699899,-0.471116428454863));
#6950=CARTESIAN_POINT('Ctrl Pts',(5.95006647750491,57.1879176050029,1.08729470798663));
#6951=CARTESIAN_POINT('Ctrl Pts',(5.76306126409791,57.1786388021573,1.83646628899214));
#6952=CARTESIAN_POINT('Ctrl Pts',(5.10503217547553,57.1592100093662,3.25130801722047));
#6953=CARTESIAN_POINT('Ctrl Pts',(4.62965976686184,57.1492324378488,3.89854020536501));
#6954=CARTESIAN_POINT('Ctrl Pts',(3.47314670683594,57.1305921723927,4.95274104346126));
#6955=CARTESIAN_POINT('Ctrl Pts',(2.80984639355393,57.1226230799194,5.35697242982361));
#6956=CARTESIAN_POINT('Ctrl Pts',(1.36281102046722,57.1045351377558,5.89420296635131));
#6957=CARTESIAN_POINT('Ctrl Pts',(0.592019886103502,57.0949002485763,6.02066309919394));
#6958=CARTESIAN_POINT('Ctrl Pts',(-0.975592711237711,57.0753050911095,5.97322267694157));
#6959=CARTESIAN_POINT('Ctrl Pts',(-1.75707259140603,57.0655365926074,5.79170805839118));
#6960=CARTESIAN_POINT('Ctrl Pts',(-3.17162316846255,57.0478547103942,5.14946248351839));
#6961=CARTESIAN_POINT('Ctrl Pts',(-3.79698591448204,57.0397273059984,4.70734163143148));
#6962=CARTESIAN_POINT('Ctrl Pts',(-4.86602922517863,57.0210198816722,3.59643623934408));
#6963=CARTESIAN_POINT('Ctrl Pts',(-5.29318280569659,57.0111540831499,2.93169004482648));
#6964=CARTESIAN_POINT('Ctrl Pts',(-5.87238998366337,56.9916557125567,1.46491314322759));
#6965=CARTESIAN_POINT('Ctrl Pts',(-6.01453244277215,56.9824032869153,0.675496041203355));
#6966=CARTESIAN_POINT('Ctrl Pts',(-5.98374780588059,56.9653602002944,-0.88110334414595));
#6967=CARTESIAN_POINT('Ctrl Pts',(-5.82343943906002,56.9562107136636,-1.63374263648686));
#6968=CARTESIAN_POINT('Ctrl Pts',(-5.21803030381155,56.9369231345048,-3.06591975237485));
#6969=CARTESIAN_POINT('Ctrl Pts',(-4.76803851417126,56.9269499412634,-3.72740099990421));
#6970=CARTESIAN_POINT('Ctrl Pts',(-3.64893183786213,56.9080665015842,-4.82566189620856));
#6971=CARTESIAN_POINT('Ctrl Pts',(-2.99515524025006,56.8999394405031,-5.25649662540572));
#6972=CARTESIAN_POINT('Ctrl Pts',(-1.56395731254144,56.8820494664067,-5.84370662915294));
#6973=CARTESIAN_POINT('Ctrl Pts',(-0.800605409757413,56.872507567622,-5.99615608358869));
#6974=CARTESIAN_POINT('Ctrl Pts',(-0.0195622404979201,56.8627445280062,
-5.99997608528796));
#6975=CARTESIAN_POINT('Ctrl Pts',(-0.00978053498370382,56.8626222566873,
-6.));
#6976=CARTESIAN_POINT('Ctrl Pts',(5.85670370643913E-14,56.8625,-6.));
#6977=CARTESIAN_POINT('Ctrl Pts',(-6.93889390390723E-16,56.806249998771,
-6.));
#6978=CARTESIAN_POINT('Ctrl Pts',(-0.648402459143038,56.8143550295102,-6.));
#6979=CARTESIAN_POINT('Ctrl Pts',(-1.29340995251398,56.8224176231774,-5.89488504120407));
#6980=CARTESIAN_POINT('Ctrl Pts',(-2.63511788894843,56.8391889723828,-5.4444243204798));
#6981=CARTESIAN_POINT('Ctrl Pts',(-3.30731393856354,56.8470979035384,-5.06431401286994));
#6982=CARTESIAN_POINT('Ctrl Pts',(-4.49746487288741,56.8655072495993,-4.05086543056204));
#6983=CARTESIAN_POINT('Ctrl Pts',(-4.99572570987037,56.8754775890921,-3.41751594850567));
#6984=CARTESIAN_POINT('Ctrl Pts',(-5.70156528953609,56.8950153414053,-2.02021237064714));
#6985=CARTESIAN_POINT('Ctrl Pts',(-5.91298550005615,56.9044034627066,-1.27503838843151));
#6986=CARTESIAN_POINT('Ctrl Pts',(-6.04518225838507,56.9219957161009,0.273740534820731));
#6987=CARTESIAN_POINT('Ctrl Pts',(-5.95722502302248,56.9305281010994,1.06331834350479));
#6988=CARTESIAN_POINT('Ctrl Pts',(-5.48124632997723,56.9497541962257,2.56454250840581));
#6989=CARTESIAN_POINT('Ctrl Pts',(-5.09742898458621,56.9596974651858,3.26146530244624));
#6990=CARTESIAN_POINT('Ctrl Pts',(-4.10086736349352,56.9787399104357,4.44516592481387));
#6991=CARTESIAN_POINT('Ctrl Pts',(-3.5059602233989,56.9874254959785,4.92796363125023));
#6992=CARTESIAN_POINT('Ctrl Pts',(-2.1369822837587,57.004537720224,5.66252364490185));
#6993=CARTESIAN_POINT('Ctrl Pts',(-1.36945084820307,57.0141318631684,5.89537543174104));
#6994=CARTESIAN_POINT('Ctrl Pts',(0.196296765378441,57.0337037083382,6.04715142045329));
#6995=CARTESIAN_POINT('Ctrl Pts',(0.978759606102301,57.0434844938472,5.97064561121902));
#6996=CARTESIAN_POINT('Ctrl Pts',(2.45446398587465,57.0619307985944,5.52775699432585));
#6997=CARTESIAN_POINT('Ctrl Pts',(3.13584909447357,57.0698632821768,5.17174421812721));
#6998=CARTESIAN_POINT('Ctrl Pts',(4.35931772271835,57.0880326402888,4.19970075246771));
#6999=CARTESIAN_POINT('Ctrl Pts',(4.88023982560178,57.097984791888,3.58111488403131));
#7000=CARTESIAN_POINT('Ctrl Pts',(5.63376775666096,57.1176123046472,2.20305247385668));
#7001=CARTESIAN_POINT('Ctrl Pts',(5.86969505471758,57.12710146791,1.46269380863545));
#7002=CARTESIAN_POINT('Ctrl Pts',(6.04992953488621,57.1448858782599,-0.0761012221813032));
#7003=CARTESIAN_POINT('Ctrl Pts',(5.98890670457258,57.1531344045418,-0.860489554575097));
#7004=CARTESIAN_POINT('Ctrl Pts',(5.56726068923777,57.1721425446805,-2.37294888625735));
#7005=CARTESIAN_POINT('Ctrl Pts',(5.20641527721435,57.1821082694806,-3.08520891385342));
#7006=CARTESIAN_POINT('Ctrl Pts',(4.24754836417997,57.2013118582877,-4.30555839024504));
#7007=CARTESIAN_POINT('Ctrl Pts',(3.66757324889836,57.2103888076896,-4.80920227021172));
#7008=CARTESIAN_POINT('Ctrl Pts',(2.32190020184786,57.2272432574316,-5.58922494954457));
#7009=CARTESIAN_POINT('Ctrl Pts',(1.56254663837337,57.2367181657913,-5.84714922855423));
#7010=CARTESIAN_POINT('Ctrl Pts',(0.517503993885004,57.2497811988474,-5.98327958263317));
#7011=CARTESIAN_POINT('Ctrl Pts',(0.258618334561658,57.2530172695889,-6.));
#7012=CARTESIAN_POINT('Ctrl Pts',(-4.9960036108132E-14,57.256249998771,
-6.));
#7013=CARTESIAN_POINT('Origin',(0.,50.,0.));
#7014=CARTESIAN_POINT('',(3.55066874434562E-14,57.7625,-6.));
#7015=CARTESIAN_POINT('',(-6.07565071524461E-15,57.706249998771,-6.));
#7016=CARTESIAN_POINT('',(-7.34788079488412E-16,50.,-6.));
#7017=CARTESIAN_POINT('Ctrl Pts',(3.67761376907083E-14,57.7625,-6.));
#7018=CARTESIAN_POINT('Ctrl Pts',(0.258110612055831,57.7592736173493,-6.));
#7019=CARTESIAN_POINT('Ctrl Pts',(0.516488526706724,57.7560438934161,-5.98334517000259));
#7020=CARTESIAN_POINT('Ctrl Pts',(1.56105720933857,57.7429867848832,-5.84754679167773));
#7021=CARTESIAN_POINT('Ctrl Pts',(2.32047460153356,57.7335085743511,-5.589816681709));
#7022=CARTESIAN_POINT('Ctrl Pts',(3.66632852427493,57.7166568288435,-4.81014823747084));
#7023=CARTESIAN_POINT('Ctrl Pts',(4.24641978670145,57.7075809259861,-4.3066680907309));
#7024=CARTESIAN_POINT('Ctrl Pts',(5.20558465828751,57.6883785712772,-3.08660464190133));
#7025=CARTESIAN_POINT('Ctrl Pts',(5.56661242618428,57.6784129776166,-2.37446201166824));
#7026=CARTESIAN_POINT('Ctrl Pts',(5.9886840232526,57.6594030932603,-0.862087265793267));
#7027=CARTESIAN_POINT('Ctrl Pts',(6.04991675977275,57.6511526636423,-0.0776590515749793));
#7028=CARTESIAN_POINT('Ctrl Pts',(5.87006062165887,57.6333697511002,1.46121605357551));
#7029=CARTESIAN_POINT('Ctrl Pts',(5.63432672297646,57.6238813508433,2.20161589450978));
#7030=CARTESIAN_POINT('Ctrl Pts',(4.88117393256969,57.6042544688462,3.57983662493059));
#7031=CARTESIAN_POINT('Ctrl Pts',(4.36042942270714,57.5943021304438,4.19854228289295));
#7032=CARTESIAN_POINT('Ctrl Pts',(3.13722222214314,57.5761308460079,5.17091463006621));
#7033=CARTESIAN_POINT('Ctrl Pts',(2.45591086078362,57.5681988857598,5.52711735424255));
#7034=CARTESIAN_POINT('Ctrl Pts',(0.980318986417133,57.5497539873302,5.97038714552931));
#7035=CARTESIAN_POINT('Ctrl Pts',(0.197896924777086,57.5399737115597,6.04709666809083));
#7036=CARTESIAN_POINT('Ctrl Pts',(-1.36787220453393,57.5204015974433,5.89574204871011));
#7037=CARTESIAN_POINT('Ctrl Pts',(-2.13546691100742,57.5108066636124,5.6630954373108));
#7038=CARTESIAN_POINT('Ctrl Pts',(-3.50463273732457,57.4936920907834,4.92890615136674));
#7039=CARTESIAN_POINT('Ctrl Pts',(-4.09966171028527,57.4850094645677,4.44627606041768));
#7040=CARTESIAN_POINT('Ctrl Pts',(-5.09652503725565,57.465968347838,3.26287235145577));
#7041=CARTESIAN_POINT('Ctrl Pts',(-5.48052530547623,57.4560253069035,2.5660762320662));
#7042=CARTESIAN_POINT('Ctrl Pts',(-5.9569427420416,57.4367974913717,1.06494645160616));
#7043=CARTESIAN_POINT('Ctrl Pts',(-6.04511867915217,57.4282624831873,0.275326005877001));
#7044=CARTESIAN_POINT('Ctrl Pts',(-5.91330773664244,57.410671789239,-1.2735316127887));
#7045=CARTESIAN_POINT('Ctrl Pts',(-5.70208388348488,57.4012845128089,-2.01874091612926));
#7046=CARTESIAN_POINT('Ctrl Pts',(-4.9966276237321,57.3817475593453,-3.41619200927743));
#7047=CARTESIAN_POINT('Ctrl Pts',(-4.49854962822897,57.3717771185393,-4.04965641382376));
#7048=CARTESIAN_POINT('Ctrl Pts',(-3.30866732480217,57.3533658829282,-5.06343463942207));
#7049=CARTESIAN_POINT('Ctrl Pts',(-2.63654373742122,57.3454567967178,-5.4437383734588));
#7050=CARTESIAN_POINT('Ctrl Pts',(-1.2944343830689,57.3286804297884,-5.89471689272042));
#7051=CARTESIAN_POINT('Ctrl Pts',(-0.648920882495232,57.3206115110312,-6.));
#7052=CARTESIAN_POINT('Ctrl Pts',(1.08385522779031E-13,57.3125,-6.));
#7053=CARTESIAN_POINT('Ctrl Pts',(-4.76008121808036E-14,57.256249998771,
-6.));
#7054=CARTESIAN_POINT('Ctrl Pts',(-0.519436872236381,57.2627429596739,-5.99999999999999));
#7055=CARTESIAN_POINT('Ctrl Pts',(-1.03779532898449,57.2692224403833,-5.93254268395134));
#7056=CARTESIAN_POINT('Ctrl Pts',(-2.27613559137132,57.2847016936631,-5.60325267671887));
#7057=CARTESIAN_POINT('Ctrl Pts',(-2.96664814970964,57.2927387106259,-5.27031552020861));
#7058=CARTESIAN_POINT('Ctrl Pts',(-4.21457381419212,57.3105680471163,-4.34380218297167));
#7059=CARTESIAN_POINT('Ctrl Pts',(-4.75210513328209,57.3203755926538,-3.74816378575814));
#7060=CARTESIAN_POINT('Ctrl Pts',(-5.5526541858912,57.3399623225271,-2.40101639440333));
#7061=CARTESIAN_POINT('Ctrl Pts',(-5.81536420644968,57.3495518110932,-1.66685308668976));
#7062=CARTESIAN_POINT('Ctrl Pts',(-6.04792418952215,57.367540960483,-0.139355216686795));
#7063=CARTESIAN_POINT('Ctrl Pts',(-6.01561379010144,57.375577236203,0.639687804988226));
#7064=CARTESIAN_POINT('Ctrl Pts',(-5.65245436363216,57.3943403650438,2.16328121029141));
#7065=CARTESIAN_POINT('Ctrl Pts',(-5.31701861410011,57.4043173426411,2.89125100224821));
#7066=CARTESIAN_POINT('Ctrl Pts',(-4.39988869026892,57.4236783666517,4.15024058173161));
#7067=CARTESIAN_POINT('Ctrl Pts',(-3.83630861676176,57.432893754617,4.67613855017113));
#7068=CARTESIAN_POINT('Ctrl Pts',(-2.51103415904724,57.4501797145846,5.5077995677353));
#7069=CARTESIAN_POINT('Ctrl Pts',(-1.75440706620821,57.4593199104434,5.79337860149726));
#7070=CARTESIAN_POINT('Ctrl Pts',(-0.190516556092516,57.4788685418198,6.04797102451951));
#7071=CARTESIAN_POINT('Ctrl Pts',(0.600273930605387,57.4887534229035,6.02112312229376));
#7072=CARTESIAN_POINT('Ctrl Pts',(2.10239675516878,57.5075299582106,5.67059173961374));
#7073=CARTESIAN_POINT('Ctrl Pts',(2.80190577330558,57.5157428591829,5.3595703237078));
#7074=CARTESIAN_POINT('Ctrl Pts',(4.07717959526911,57.5333107146008,4.47300103937156));
#7075=CARTESIAN_POINT('Ctrl Pts',(4.63295849576113,57.5430472346991,3.89445893722693));
#7076=CARTESIAN_POINT('Ctrl Pts',(5.47632776170528,57.5626446916676,2.57104288095419));
#7077=CARTESIAN_POINT('Ctrl Pts',(5.76225600572969,57.5723124689847,1.84305261576839));
#7078=CARTESIAN_POINT('Ctrl Pts',(6.04013983523531,57.5904750269888,0.325703679081649));
#7079=CARTESIAN_POINT('Ctrl Pts',(6.03222718366437,57.5984092303024,-0.44900774578563));
#7080=CARTESIAN_POINT('Ctrl Pts',(5.71911276192995,57.6169547111498,-1.98138918762898));
#7081=CARTESIAN_POINT('Ctrl Pts',(5.40594485041393,57.6269305930548,-2.72211410612992));
#7082=CARTESIAN_POINT('Ctrl Pts',(4.52573222705394,57.6464069267401,-4.01306975045855));
#7083=CARTESIAN_POINT('Ctrl Pts',(3.97684854565217,57.6557321097956,-4.55759512082249));
#7084=CARTESIAN_POINT('Ctrl Pts',(2.6826884329283,57.6732100113963,-5.4249508224125));
#7085=CARTESIAN_POINT('Ctrl Pts',(1.94417005043746,57.6819478731405,-5.73124160488625));
#7086=CARTESIAN_POINT('Ctrl Pts',(0.782107764040655,57.6964736517205,-5.96176932725523));
#7087=CARTESIAN_POINT('Ctrl Pts',(0.391053241759171,57.701361833249,-6.));
#7088=CARTESIAN_POINT('Ctrl Pts',(-1.94289029309402E-15,57.706249998771,
-6.));
#7089=CARTESIAN_POINT('Origin',(0.,50.,0.));
#7090=CARTESIAN_POINT('',(-1.93563819391985E-14,58.2125,-6.));
#7091=CARTESIAN_POINT('',(-1.96575190926063E-14,58.156249998771,-6.));
#7092=CARTESIAN_POINT('',(-7.34788079488412E-16,50.,-6.));
#7093=CARTESIAN_POINT('Ctrl Pts',(-7.84095011141517E-15,58.2125,-6.));
#7094=CARTESIAN_POINT('Ctrl Pts',(0.390457421837537,58.207619282227,-6.));
#7095=CARTESIAN_POINT('Ctrl Pts',(0.780918842935951,58.2027385144633,-5.96188574511026));
#7096=CARTESIAN_POINT('Ctrl Pts',(1.94253419381023,58.1882183225773,-5.73180637727347));
#7097=CARTESIAN_POINT('Ctrl Pts',(2.681207844968,58.1794773050473,-5.42569341007508));
#7098=CARTESIAN_POINT('Ctrl Pts',(3.97563925209768,58.1620010529719,-4.55864671700234));
#7099=CARTESIAN_POINT('Ctrl Pts',(4.52465365959551,58.1526767919982,-4.01428199965563));
#7100=CARTESIAN_POINT('Ctrl Pts',(5.40519277828591,58.1332013855122,-2.72360050849763));
#7101=CARTESIAN_POINT('Ctrl Pts',(5.71855682515151,58.1232254511625,-1.98298398415952));
#7102=CARTESIAN_POINT('Ctrl Pts',(6.03210756855281,58.1046780422682,-0.450676347406313));
#7103=CARTESIAN_POINT('Ctrl Pts',(6.04023242288917,58.0967432727997,0.324071772308548));
#7104=CARTESIAN_POINT('Ctrl Pts',(5.76274605643686,58.0785822192762,1.84151120643125));
#7105=CARTESIAN_POINT('Ctrl Pts',(5.47702135089854,58.0689150927559,2.56955886657416));
#7106=CARTESIAN_POINT('Ctrl Pts',(4.6340254354337,58.0493176466484,3.89318947355464));
#7107=CARTESIAN_POINT('Ctrl Pts',(4.07840450937353,58.0395804601485,4.47188434182551));
#7108=CARTESIAN_POINT('Ctrl Pts',(2.8033690403144,58.0220102826005,5.35880574845981));
#7109=CARTESIAN_POINT('Ctrl Pts',(2.10394053493841,58.0137992566867,5.6700197498057));
#7110=CARTESIAN_POINT('Ctrl Pts',(0.601929482491991,57.9950241185311,6.02095503373109));
#7111=CARTESIAN_POINT('Ctrl Pts',(-0.188831349820596,57.9851396081272,6.04802107703606));
#7112=CARTESIAN_POINT('Ctrl Pts',(-1.75284859095268,57.9655893926131,5.79386100479629));
#7113=CARTESIAN_POINT('Ctrl Pts',(-2.50962521800312,57.9564455943931,5.50845291559488));
#7114=CARTESIAN_POINT('Ctrl Pts',(-3.8351523571085,57.939161216313,4.67708391219656));
#7115=CARTESIAN_POINT('Ctrl Pts',(-4.39884929925911,57.9299467530942,4.15133884232404));
#7116=CARTESIAN_POINT('Ctrl Pts',(-5.31627458475805,57.9105867392603,2.8926131061046));
#7117=CARTESIAN_POINT('Ctrl Pts',(-5.65188924961675,57.9006097933443,2.16474953755615));
#7118=CARTESIAN_POINT('Ctrl Pts',(-6.01545511766878,57.8818449263436,0.641230227077598));
#7119=CARTESIAN_POINT('Ctrl Pts',(-6.0479642230219,57.8738075178057,-0.137848943610883));
#7120=CARTESIAN_POINT('Ctrl Pts',(-5.81577020278541,57.8558197836008,-1.66542737316983));
#7121=CARTESIAN_POINT('Ctrl Pts',(-5.55324765720755,57.8462309602226,-2.39963747219516));
#7122=CARTESIAN_POINT('Ctrl Pts',(-4.75304623800897,57.8266443944227,-3.7469704133501));
#7123=CARTESIAN_POINT('Ctrl Pts',(-4.21566411034092,57.8168363161938,-4.34274415418793));
#7124=CARTESIAN_POINT('Ctrl Pts',(-2.96796066775887,57.7990048960901,-5.26957826725007));
#7125=CARTESIAN_POINT('Ctrl Pts',(-2.27751928872034,57.790968991109,-5.60269206319514));
#7126=CARTESIAN_POINT('Ctrl Pts',(-1.03877270146848,57.7754846587683,-5.93241487607021));
#7127=CARTESIAN_POINT('Ctrl Pts',(-0.519928662438415,57.7689991082805,-6.));
#7128=CARTESIAN_POINT('Ctrl Pts',(8.11850586757146E-14,57.7625,-6.));
#7129=CARTESIAN_POINT('Ctrl Pts',(-1.28369537222284E-14,57.706249998771,
-6.));
#7130=CARTESIAN_POINT('Ctrl Pts',(-0.391601361600674,57.711145015791,-6.));
#7131=CARTESIAN_POINT('Ctrl Pts',(-0.783201439086809,57.7160400167596,-5.96166207261296));
#7132=CARTESIAN_POINT('Ctrl Pts',(-1.91335725960868,57.7301669645161,-5.73714195665658));
#7133=CARTESIAN_POINT('Ctrl Pts',(-2.62281749872555,57.73865054735,-5.44945314815992));
#7134=CARTESIAN_POINT('Ctrl Pts',(-3.92669804958441,57.7559342308597,-4.60565064288469));
#7135=CARTESIAN_POINT('Ctrl Pts',(-4.50127582338596,57.7655845989079,-4.04592046079129));
#7136=CARTESIAN_POINT('Ctrl Pts',(-5.38942554973876,57.7851724256882,-2.74924801407657));
#7137=CARTESIAN_POINT('Ctrl Pts',(-5.69991244388084,57.7949140509847,-2.02861490802512));
#7138=CARTESIAN_POINT('Ctrl Pts',(-6.02580821468928,57.813256188233,-0.52239685858074));
#7139=CARTESIAN_POINT('Ctrl Pts',(-6.04332107158197,57.821164533169,0.248056565886231));
#7140=CARTESIAN_POINT('Ctrl Pts',(-5.78257606509501,57.839474882712,1.78895300421315));
#7141=CARTESIAN_POINT('Ctrl Pts',(-5.49318999140679,57.8494389828867,2.54232002356862));
#7142=CARTESIAN_POINT('Ctrl Pts',(-4.65273329361551,57.8690165395379,3.86557933928005));
#7143=CARTESIAN_POINT('Ctrl Pts',(-4.11986225783113,57.8784478281965,4.42915123066452));
#7144=CARTESIAN_POINT('Ctrl Pts',(-2.85826880174532,57.8961207399164,5.3333235633937));
#7145=CARTESIAN_POINT('Ctrl Pts',(-2.13805071417483,57.9045243648438,5.6606351502864));
#7146=CARTESIAN_POINT('Ctrl Pts',(-0.607167279468976,57.9236604077776,6.02113734956474));
#7147=CARTESIAN_POINT('Ctrl Pts',(0.189158021930711,57.9336144740451,6.04871588527682));
#7148=CARTESIAN_POINT('Ctrl Pts',(1.71801944063456,57.9527252417789,5.79879535798965));
#7149=CARTESIAN_POINT('Ctrl Pts',(2.43798162431586,57.9615715966977,5.53478334131579));
#7150=CARTESIAN_POINT('Ctrl Pts',(3.77031407405033,57.9785619662946,4.73450272615289));
#7151=CARTESIAN_POINT('Ctrl Pts',(4.36322000407077,57.9881143046535,4.19440990478975));
#7152=CARTESIAN_POINT('Ctrl Pts',(5.29575070535321,58.007670328558,2.92629864971634));
#7153=CARTESIAN_POINT('Ctrl Pts',(5.63087522327058,58.0174765634655,2.21392170217679));
#7154=CARTESIAN_POINT('Ctrl Pts',(6.00512131537034,58.0359950673901,0.719326668055239));
#7155=CARTESIAN_POINT('Ctrl Pts',(6.04786576453849,58.0439618266081,-0.0472031294460459));
#7156=CARTESIAN_POINT('Ctrl Pts',(5.83917914624789,58.0620314364426,-1.59591691053384));
#7157=CARTESIAN_POINT('Ctrl Pts',(5.57387686409125,58.0719730483531,-2.3611113365425));
#7158=CARTESIAN_POINT('Ctrl Pts',(4.77400611905593,58.0916313179331,-3.71525890399387));
#7159=CARTESIAN_POINT('Ctrl Pts',(4.25766524315068,58.1011589707271,-4.29727622515334));
#7160=CARTESIAN_POINT('Ctrl Pts',(3.02845794881133,58.1190200122784,-5.23752540649854));
#7161=CARTESIAN_POINT('Ctrl Pts',(2.32577158057442,58.1271778540138,-5.58516084716442));
#7162=CARTESIAN_POINT('Ctrl Pts',(1.06150779516445,58.1429811513315,-5.92941344534358));
#7163=CARTESIAN_POINT('Ctrl Pts',(0.53134688384117,58.1496081627229,-6.));
#7164=CARTESIAN_POINT('Ctrl Pts',(-6.77236045021345E-14,58.156249998771,
-6.));
#7165=CARTESIAN_POINT('Origin',(0.,50.,0.));
#7166=CARTESIAN_POINT('',(7.61233394974911E-15,58.6625,-6.));
#7167=CARTESIAN_POINT('',(-2.14616315076222E-14,58.606249998771,-6.));
#7168=CARTESIAN_POINT('',(-7.34788079488412E-16,50.,-6.));
#7169=CARTESIAN_POINT('Ctrl Pts',(6.38378239159465E-14,58.6625,-6.));
#7170=CARTESIAN_POINT('Ctrl Pts',(0.530776948296579,58.6558652881463,-6.));
#7171=CARTESIAN_POINT('Ctrl Pts',(1.06037530332947,58.6492453087083,-5.92956480662758));
#7172=CARTESIAN_POINT('Ctrl Pts',(2.32423742973157,58.6334470321283,-5.58580676470304));
#7173=CARTESIAN_POINT('Ctrl Pts',(3.02706636248606,58.6252875032083,-5.23833760312848));
#7174=CARTESIAN_POINT('Ctrl Pts',(4.25654205503151,58.6074279973176,-4.2983852398153));
#7175=CARTESIAN_POINT('Ctrl Pts',(4.7730223061995,58.597901105114,-3.71651864733174));
#7176=CARTESIAN_POINT('Ctrl Pts',(5.57323346422887,58.5782434223283,-2.36262182315155));
#7177=CARTESIAN_POINT('Ctrl Pts',(5.83873697489378,58.5683015800684,-1.59752229770145));
#7178=CARTESIAN_POINT('Ctrl Pts',(6.04785491129762,58.5502299481763,-0.0488707485619556));
#7179=CARTESIAN_POINT('Ctrl Pts',(6.00531951855148,58.5422640224442,0.717690221353016));
#7180=CARTESIAN_POINT('Ctrl Pts',(5.63147665457864,58.5237469701109,2.21238396707949));
#7181=CARTESIAN_POINT('Ctrl Pts',(5.29655706242653,58.5139412327658,2.92483326571615));
#7182=CARTESIAN_POINT('Ctrl Pts',(4.3643932130471,58.4943848513782,4.19318934571028));
#7183=CARTESIAN_POINT('Ctrl Pts',(3.77163749598118,58.4848316490538,4.73344870227629));
#7184=CARTESIAN_POINT('Ctrl Pts',(2.43954091256409,58.4678388044587,5.53409412546177));
#7185=CARTESIAN_POINT('Ctrl Pts',(1.71966841461828,58.4589958551827,5.79830452948859));
#7186=CARTESIAN_POINT('Ctrl Pts',(0.190917060146435,58.4398864632518,6.04865757988973));
#7187=CARTESIAN_POINT('Ctrl Pts',(-0.605392310407389,58.4299325961199,6.02131301640874));
#7188=CARTESIAN_POINT('Ctrl Pts',(-2.13642329321222,58.4107947088348,5.66125848153069));
#7189=CARTESIAN_POINT('Ctrl Pts',(-2.85679415977466,58.4023886124107,5.33412305523624));
#7190=CARTESIAN_POINT('Ctrl Pts',(-4.11866454336098,58.3847173340954,4.43026149411868));
#7191=CARTESIAN_POINT('Ctrl Pts',(-4.65167436976604,58.3752869090688,3.8668495124502));
#7192=CARTESIAN_POINT('Ctrl Pts',(-5.49247371789428,58.3557101285827,2.54385972506567));
#7193=CARTESIAN_POINT('Ctrl Pts',(-5.78206393462196,58.3457458823708,1.7905970774123));
#7194=CARTESIAN_POINT('Ctrl Pts',(-6.04325418504873,58.3274335033081,0.249770221784229));
#7195=CARTESIAN_POINT('Ctrl Pts',(-6.02595721866325,58.3195252934994,-0.520718130671191));
#7196=CARTESIAN_POINT('Ctrl Pts',(-5.70047225331914,58.30118467433,-2.02703312465037));
#7197=CARTESIAN_POINT('Ctrl Pts',(-5.39019517581812,58.2914436403568,-2.74773274428987));
#7198=CARTESIAN_POINT('Ctrl Pts',(-4.50242576317489,58.271855638718,-4.04464091796179));
#7199=CARTESIAN_POINT('Ctrl Pts',(-3.92800637799208,58.2622044860682,-4.60453502415897));
#7200=CARTESIAN_POINT('Ctrl Pts',(-2.62436906678792,58.2449183407013,-5.44870538053932));
#7201=CARTESIAN_POINT('Ctrl Pts',(-1.91499593268198,58.2364374491585,-5.73659449375919));
#7202=CARTESIAN_POINT('Ctrl Pts',(-0.784344980001046,58.22230431225,-5.96154976010922));
#7203=CARTESIAN_POINT('Ctrl Pts',(-0.392174507256861,58.2174021813407,-6.));
#7204=CARTESIAN_POINT('Ctrl Pts',(1.45716771982052E-14,58.2125,-6.));
#7205=CARTESIAN_POINT('Ctrl Pts',(-5.02375918642883E-14,58.156249998771,
-6.));
#7206=CARTESIAN_POINT('Ctrl Pts',(-0.25714894131831,58.1594643605374,-6.));
#7207=CARTESIAN_POINT('Ctrl Pts',(-0.514575654230465,58.1626821944489,-5.9834690716322));
#7208=CARTESIAN_POINT('Ctrl Pts',(-1.5265971378732,58.1753324629944,-5.85239233164468));
#7209=CARTESIAN_POINT('Ctrl Pts',(-2.25698495692498,58.1844623107326,-5.6113307664574));
#7210=CARTESIAN_POINT('Ctrl Pts',(-3.61632703393217,58.2014540866952,-4.85314392082562));
#7211=CARTESIAN_POINT('Ctrl Pts',(-4.22630969876986,58.2107654711745,-4.33234064579157));
#7212=CARTESIAN_POINT('Ctrl Pts',(-5.20060604096146,58.2302727419895,-3.09284641223551));
#7213=CARTESIAN_POINT('Ctrl Pts',(-5.5591352207356,58.2401313235473,-2.38914657610037));
#7214=CARTESIAN_POINT('Ctrl Pts',(-5.9795861406248,58.2588139326938,-0.906068520694137));
#7215=CARTESIAN_POINT('Ctrl Pts',(-6.04615338414096,58.2669142064327,-0.142936563359255));
#7216=CARTESIAN_POINT('Ctrl Pts',(-5.88759600211521,58.2846366202039,1.40264674728406));
#7217=CARTESIAN_POINT('Ctrl Pts',(-5.65034250025109,58.2944161144496,2.16905935577278));
#7218=CARTESIAN_POINT('Ctrl Pts',(-4.9011161956024,58.314009575749,3.54645977198778));
#7219=CARTESIAN_POINT('Ctrl Pts',(-4.40357509149157,58.3236323117353,4.14811455551955));
#7220=CARTESIAN_POINT('Ctrl Pts',(-3.2099264188501,58.3416933616046,5.1273694936731));
#7221=CARTESIAN_POINT('Ctrl Pts',(-2.52572795615392,58.3496783993191,5.49674864765797));
#7222=CARTESIAN_POINT('Ctrl Pts',(-1.03180736684294,58.3683524066855,5.96381579552218));
#7223=CARTESIAN_POINT('Ctrl Pts',(-0.233589182840623,58.3783301339855,6.04790490889298));
#7224=CARTESIAN_POINT('Ctrl Pts',(1.31928168112156,58.3977410197851,5.90291812233691));
#7225=CARTESIAN_POINT('Ctrl Pts',(2.06022289020428,58.4070027848986,5.68686607011341));
#7226=CARTESIAN_POINT('Ctrl Pts',(3.44950256049131,58.4243687807772,4.97352571573904));
#7227=CARTESIAN_POINT('Ctrl Pts',(4.07883956806913,58.4333327305947,4.47192567472073));
#7228=CARTESIAN_POINT('Ctrl Pts',(5.09696837341051,58.4528001027957,3.26142380164731));
#7229=CARTESIAN_POINT('Ctrl Pts',(5.47942654470292,58.4627028299152,2.56746138288995));
#7230=CARTESIAN_POINT('Ctrl Pts',(5.9474986674038,58.4815497550765,1.09669857848434));
#7231=CARTESIAN_POINT('Ctrl Pts',(6.03838547141748,58.4898651117374,0.336708629691644));
#7232=CARTESIAN_POINT('Ctrl Pts',(5.92966814879028,58.5073150461233,-1.21247928523865));
#7233=CARTESIAN_POINT('Ctrl Pts',(5.71722611244321,58.5170169126582,-1.98604585925342));
#7234=CARTESIAN_POINT('Ctrl Pts',(5.01170895965484,58.5366129890372,-3.38892333677217));
#7235=CARTESIAN_POINT('Ctrl Pts',(4.53192741509464,58.5463127945614,-4.00795098574795));
#7236=CARTESIAN_POINT('Ctrl Pts',(3.37083052662181,58.5645509502237,-5.02236003761031));
#7237=CARTESIAN_POINT('Ctrl Pts',(2.70287198424826,58.5724640989679,-5.41119964526751));
#7238=CARTESIAN_POINT('Ctrl Pts',(1.34267769100579,58.5894665276335,-5.88666693746568));
#7239=CARTESIAN_POINT('Ctrl Pts',(0.673269435414399,58.5978341308283,-6.));
#7240=CARTESIAN_POINT('Ctrl Pts',(-9.29811783123569E-15,58.606249998771,
-6.));
#7241=CARTESIAN_POINT('Origin',(0.,50.,0.));
#7242=CARTESIAN_POINT('',(-8.76345566347195E-15,59.1125,-6.));
#7243=CARTESIAN_POINT('',(-2.67351908745917E-14,59.056249998771,-6.));
#7244=CARTESIAN_POINT('',(-7.34788079488412E-16,50.,-6.));
#7245=CARTESIAN_POINT('Ctrl Pts',(-4.9960036108132E-15,59.1125,-6.));
#7246=CARTESIAN_POINT('Ctrl Pts',(0.672701052867484,59.1040912368392,-6.));
#7247=CARTESIAN_POINT('Ctrl Pts',(1.34155536469756,59.0957305579412,-5.88685820339337));
#7248=CARTESIAN_POINT('Ctrl Pts',(2.70138297915581,59.0787327127605,-5.41194792946457));
#7249=CARTESIAN_POINT('Ctrl Pts',(3.36947757384086,59.0708192903467,-5.02327298442946));
#7250=CARTESIAN_POINT('Ctrl Pts',(4.53085258097578,59.0525826236427,-4.00916204852835));
#7251=CARTESIAN_POINT('Ctrl Pts',(5.01078795041768,59.0428834359837,-3.39028028632475));
#7252=CARTESIAN_POINT('Ctrl Pts',(5.71668122894584,59.0232872955114,-1.98761404442142));
#7253=CARTESIAN_POINT('Ctrl Pts',(5.92933561133885,59.0135847241384,-1.21410495830013));
#7254=CARTESIAN_POINT('Ctrl Pts',(6.03847755750431,58.996132443645,0.335054524239836));
#7255=CARTESIAN_POINT('Ctrl Pts',(5.94779882789026,58.9878192630031,1.09506992468099));
#7256=CARTESIAN_POINT('Ctrl Pts',(5.48013577684982,58.9689737276042,2.5659405259635));
#7257=CARTESIAN_POINT('Ctrl Pts',(5.09788218678483,58.9590713368697,3.25998998583337));
#7258=CARTESIAN_POINT('Ctrl Pts',(4.08006393409214,58.9396023325235,4.47082192767438));
#7259=CARTESIAN_POINT('Ctrl Pts',(3.4508003450447,58.930635004313,4.97263730701852));
#7260=CARTESIAN_POINT('Ctrl Pts',(2.06164762259643,58.9132705952824,5.68634721117428));
#7261=CARTESIAN_POINT('Ctrl Pts',(1.32077933349314,58.9040097416686,5.90258078485799));
#7262=CARTESIAN_POINT('Ctrl Pts',(-0.23201437723163,58.8845998202845,6.04796271876271));
#7263=CARTESIAN_POINT('Ctrl Pts',(-1.030232689666,58.8746220913791,5.96408516844816));
#7264=CARTESIAN_POINT('Ctrl Pts',(-2.52429644274422,58.8559462944656,5.49741187861185));
#7265=CARTESIAN_POINT('Ctrl Pts',(-3.20862663585613,58.8479603586346,5.12818906846544));
#7266=CARTESIAN_POINT('Ctrl Pts',(-4.4025341469145,58.8299007399992,4.14921578246961));
#7267=CARTESIAN_POINT('Ctrl Pts',(-4.90021442968027,58.8202786551822,3.54770150620519));
#7268=CARTESIAN_POINT('Ctrl Pts',(-5.64978560785529,58.8006852968284,2.17050971252699));
#7269=CARTESIAN_POINT('Ctrl Pts',(-5.8872359780719,58.7909052251381,1.40415742399703));
#7270=CARTESIAN_POINT('Ctrl Pts',(-6.04619079040954,58.7731806625371,-0.141394930549601));
#7271=CARTESIAN_POINT('Ctrl Pts',(-5.97981672468023,58.7650817790603,-0.904553185256946));
#7272=CARTESIAN_POINT('Ctrl Pts',(-5.55974238367077,58.7464004891878,-2.38772678926996));
#7273=CARTESIAN_POINT('Ctrl Pts',(-5.20140327459709,58.7365422966134,-3.0915004300368));
#7274=CARTESIAN_POINT('Ctrl Pts',(-4.22744511984234,58.7170345666816,-4.33123232759352));
#7275=CARTESIAN_POINT('Ctrl Pts',(-3.61760080633883,58.7077200100792,-4.85219413907));
#7276=CARTESIAN_POINT('Ctrl Pts',(-2.25847727368889,58.690730965921,-5.61072762006748));
#7277=CARTESIAN_POINT('Ctrl Pts',(-1.52817325669471,58.6816021657086,-5.85197840613562));
#7278=CARTESIAN_POINT('Ctrl Pts',(-0.515664031273792,58.6689458003909,-5.98339903275881));
#7279=CARTESIAN_POINT('Ctrl Pts',(-0.257693111406946,58.6657211638926,-6.));
#7280=CARTESIAN_POINT('Ctrl Pts',(5.77315972805081E-14,58.6625,-6.));
#7281=CARTESIAN_POINT('Ctrl Pts',(-8.6389229103645E-15,58.606249998771,
-6.));
#7282=CARTESIAN_POINT('Ctrl Pts',(-0.122167840796238,58.6077770967809,-6.));
#7283=CARTESIAN_POINT('Ctrl Pts',(-0.24446281392826,58.6093057839451,-5.99626881492867));
#7284=CARTESIAN_POINT('Ctrl Pts',(-1.13242499823765,58.620405311249,-5.94189557440023));
#7285=CARTESIAN_POINT('Ctrl Pts',(-1.88209003706895,58.6297761242344,-5.74858786203242));
#7286=CARTESIAN_POINT('Ctrl Pts',(-3.286925598113,58.6473365687475,-5.08108066159058));
#7287=CARTESIAN_POINT('Ctrl Pts',(-3.9252649774435,58.655923449754,-4.60581917418637));
#7288=CARTESIAN_POINT('Ctrl Pts',(-4.98122649564737,58.6751844809384,-3.43622099470862));
#7289=CARTESIAN_POINT('Ctrl Pts',(-5.38876716441984,58.6851229553633,-2.75343776800202));
#7290=CARTESIAN_POINT('Ctrl Pts',(-5.90728745868403,58.7041382468853,-1.29624821084482));
#7291=CARTESIAN_POINT('Ctrl Pts',(-6.02374820107787,58.7127645881171,-0.539197522072843));
#7292=CARTESIAN_POINT('Ctrl Pts',(-5.96693876608166,58.7299246617597,1.01318323723523));
#7293=CARTESIAN_POINT('Ctrl Pts',(-5.7805594195143,58.7395348055697,1.7933241298239));
#7294=CARTESIAN_POINT('Ctrl Pts',(-5.12147213884938,58.7591118583213,3.22125057908729));
#7295=CARTESIAN_POINT('Ctrl Pts',(-4.66080840540443,58.7688821135053,3.85782376226492));
#7296=CARTESIAN_POINT('Ctrl Pts',(-3.53381833581784,58.7872996547863,4.90849532883619));
#7297=CARTESIAN_POINT('Ctrl Pts',(-2.88219839217209,58.7952225188689,5.31734221965164));
#7298=CARTESIAN_POINT('Ctrl Pts',(-1.42550782171891,58.8134311509996,5.88288560888607));
#7299=CARTESIAN_POINT('Ctrl Pts',(-0.629041201384563,58.8233869837537,6.02035799191243));
#7300=CARTESIAN_POINT('Ctrl Pts',(0.940108615079224,58.8430013564595,5.97564886933408));
#7301=CARTESIAN_POINT('Ctrl Pts',(1.69798518433907,58.8524748135753,5.80594902646743));
#7302=CARTESIAN_POINT('Ctrl Pts',(3.11828402566099,58.8702285490918,5.1851233141816));
#7303=CARTESIAN_POINT('Ctrl Pts',(3.76563250801836,58.878517043524,4.73594961054287));
#7304=CARTESIAN_POINT('Ctrl Pts',(4.85877481455106,58.8975607639645,3.60789207585319));
#7305=CARTESIAN_POINT('Ctrl Pts',(5.29123706747589,58.9075236638755,2.93724100270947));
#7306=CARTESIAN_POINT('Ctrl Pts',(5.86054611470443,58.9267020894045,1.49430467168795));
#7307=CARTESIAN_POINT('Ctrl Pts',(6.00262912888888,58.9357246929159,0.739828071058013));
#7308=CARTESIAN_POINT('Ctrl Pts',(5.99718050207131,58.9525922230467,-0.815181852638874));
#7309=CARTESIAN_POINT('Ctrl Pts',(5.83675262210175,58.9621009230984,-1.60093485847068));
#7310=CARTESIAN_POINT('Ctrl Pts',(5.22441553448639,58.9816373541801,-3.05210007514069));
#7311=CARTESIAN_POINT('Ctrl Pts',(4.7832531634121,58.9914672910168,-3.70544553004886));
#7312=CARTESIAN_POINT('Ctrl Pts',(3.69023259964329,59.0100570779767,-4.79164077420985));
#7313=CARTESIAN_POINT('Ctrl Pts',(3.05422553412945,59.0180721795944,-5.22008986623226));
#7314=CARTESIAN_POINT('Ctrl Pts',(1.62445341044163,59.0359443311405,-5.83030169809409));
#7315=CARTESIAN_POINT('Ctrl Pts',(0.838982768159112,59.0457627141691,-5.99394362288408));
#7316=CARTESIAN_POINT('Ctrl Pts',(0.0296581642327382,59.0558792717181,-5.99994503405408));
#7317=CARTESIAN_POINT('Ctrl Pts',(0.0148278070826941,59.0560646511824,-6.));
#7318=CARTESIAN_POINT('Ctrl Pts',(-5.65218389446823E-14,59.056249998771,
-6.));
#7319=CARTESIAN_POINT('Origin',(0.,50.,0.));
#7320=CARTESIAN_POINT('',(-6.82056537037793E-15,59.5625,-6.));
#7321=CARTESIAN_POINT('',(-1.86166850070202E-14,59.506249998771,-6.));
#7322=CARTESIAN_POINT('',(-7.34788079488412E-16,50.,-6.));
#7323=CARTESIAN_POINT('Ctrl Pts',(-5.67635441770116E-14,59.5625,-6.));
#7324=CARTESIAN_POINT('Ctrl Pts',(0.0142972269403468,59.5623212846632,-6.));
#7325=CARTESIAN_POINT('Ctrl Pts',(0.0285968282160099,59.5621425396472,-5.9999488973426));
#7326=CARTESIAN_POINT('Ctrl Pts',(0.837392612400114,59.5520325923449,-5.9941660570088));
#7327=CARTESIAN_POINT('Ctrl Pts',(1.62290717636517,59.5422136602954,-5.83073236561579));
#7328=CARTESIAN_POINT('Ctrl Pts',(3.05285476740338,59.5243393154074,-5.22089374457676));
#7329=CARTESIAN_POINT('Ctrl Pts',(3.68898612233827,59.5163252834728,-4.79260275836969));
#7330=CARTESIAN_POINT('Ctrl Pts',(4.78228266676363,59.4977368696895,-3.7066937003491));
#7331=CARTESIAN_POINT('Ctrl Pts',(5.22360516457189,59.4879073757064,-3.05348160371385));
#7332=CARTESIAN_POINT('Ctrl Pts',(5.83632373739268,59.4683705289908,-1.60249824301388));
#7333=CARTESIAN_POINT('Ctrl Pts',(5.99696223601562,59.4588609656099,-0.816787086981186));
#7334=CARTESIAN_POINT('Ctrl Pts',(6.0028267344566,59.4419910447185,0.738203582127298));
#7335=CARTESIAN_POINT('Ctrl Pts',(5.86095264654097,59.4329720056696,1.4926997107051));
#7336=CARTESIAN_POINT('Ctrl Pts',(5.29205835188024,59.4137948851477,2.93575494784605));
#7337=CARTESIAN_POINT('Ctrl Pts',(4.85979813697018,59.4038321375293,3.60650859949935));
#7338=CARTESIAN_POINT('Ctrl Pts',(3.7669558879038,59.3847866057346,4.73490669818668));
#7339=CARTESIAN_POINT('Ctrl Pts',(3.11968095784071,59.3764960119729,5.18429174793231));
#7340=CARTESIAN_POINT('Ctrl Pts',(1.69950759641262,59.3587438449551,5.80550095706382));
#7341=CARTESIAN_POINT('Ctrl Pts',(0.941695634254267,59.3492711954281,5.97539643738251));
#7342=CARTESIAN_POINT('Ctrl Pts',(-0.627399432048698,59.3296575070993,6.02052625534498));
#7343=CARTESIAN_POINT('Ctrl Pts',(-1.42388046024521,59.3197014942469,5.88327657912861));
#7344=CARTESIAN_POINT('Ctrl Pts',(-2.88073088984782,59.3014908638768,5.31814090999649));
#7345=CARTESIAN_POINT('Ctrl Pts',(-3.53248421704506,59.293568429975,4.90945933911823));
#7346=CARTESIAN_POINT('Ctrl Pts',(-4.65975855504601,59.2751523573231,3.85908756114137));
#7347=CARTESIAN_POINT('Ctrl Pts',(-5.12058362693479,59.2653826456766,3.22265773660764));
#7348=CARTESIAN_POINT('Ctrl Pts',(-5.78006018634094,59.2458053434966,1.79493299632178));
#7349=CARTESIAN_POINT('Ctrl Pts',(-5.96665683265347,59.2361943925425,1.01484300101855));
#7350=CARTESIAN_POINT('Ctrl Pts',(-6.02389751968685,59.2190318862247,-0.537513495724967));
#7351=CARTESIAN_POINT('Ctrl Pts',(-5.90765047541225,59.21040849796,-1.29458719801825));
#7352=CARTESIAN_POINT('Ctrl Pts',(-5.38955293821489,59.1913945918115,-2.75189285876347));
#7353=CARTESIAN_POINT('Ctrl Pts',(-4.98222117445791,59.181456369504,-3.4347734072283));
#7354=CARTESIAN_POINT('Ctrl Pts',(-3.92657290615344,59.162193568645,-4.60471591715926));
#7355=CARTESIAN_POINT('Ctrl Pts',(-3.28830864106957,59.1536038580133,-5.08019633894838));
#7356=CARTESIAN_POINT('Ctrl Pts',(-1.88360262186521,59.1360450327733,-5.74808979396372));
#7357=CARTESIAN_POINT('Ctrl Pts',(-1.13400840618302,59.1266751050772,-5.94159104245208));
#7358=CARTESIAN_POINT('Ctrl Pts',(-0.245540622028225,59.1155692577753,-5.99623585121819));
#7359=CARTESIAN_POINT('Ctrl Pts',(-0.122706315052604,59.1140338289381,-6.));
#7360=CARTESIAN_POINT('Ctrl Pts',(2.15105711021124E-15,59.1125,-6.));
#7361=CARTESIAN_POINT('Ctrl Pts',(-6.89726054048379E-14,59.056249998771,
-6.));
#7362=CARTESIAN_POINT('Ctrl Pts',(-0.757078466779825,59.0657134796057,-5.99999999999999));
#7363=CARTESIAN_POINT('Ctrl Pts',(-1.5075091086108,59.0750938626287,-5.85670543582169));
#7364=CARTESIAN_POINT('Ctrl Pts',(-2.93051707960641,59.0928814622661,-5.29247310863984));
#7365=CARTESIAN_POINT('Ctrl Pts',(-3.58763195986761,59.1009420642367,-4.87104734369159));
#7366=CARTESIAN_POINT('Ctrl Pts',(-4.72000389175098,59.1197409195129,-3.78825871871639));
#7367=CARTESIAN_POINT('Ctrl Pts',(-5.17898245154283,59.1297171122548,-3.13168890336551));
#7368=CARTESIAN_POINT('Ctrl Pts',(-5.80297691642877,59.1490570771964,-1.70540284121377));
#7369=CARTESIAN_POINT('Ctrl Pts',(-5.97269404694987,59.1582532989466,-0.953878495726881));
#7370=CARTESIAN_POINT('Ctrl Pts',(-6.02247403535284,59.1755065785828,0.611170717347984));
#7371=CARTESIAN_POINT('Ctrl Pts',(-5.8868748344451,59.1847221165161,1.4101281919661));
#7372=CARTESIAN_POINT('Ctrl Pts',(-5.31637666959674,59.2043033009837,2.88958326266276));
#7373=CARTESIAN_POINT('Ctrl Pts',(-4.89414615252563,59.2141803842959,3.55821423342768));
#7374=CARTESIAN_POINT('Ctrl Pts',(-3.83345597946988,59.2329280106712,4.67765601799604));
#7375=CARTESIAN_POINT('Ctrl Pts',(-3.21173159001649,59.2411033538958,5.12451161277228));
#7376=CARTESIAN_POINT('Ctrl Pts',(-1.80247080507788,59.2587191137075,5.77773781424917));
#7377=CARTESIAN_POINT('Ctrl Pts',(-1.02245955129053,59.2684692543798,5.96537636458588));
#7378=CARTESIAN_POINT('Ctrl Pts',(0.545294980710786,59.2880661860299,6.0251496297033));
#7379=CARTESIAN_POINT('Ctrl Pts',(1.31763040516511,59.2977203788355,5.90454359843958));
#7380=CARTESIAN_POINT('Ctrl Pts',(2.7681420431286,59.3158517743101,5.37847456800289));
#7381=CARTESIAN_POINT('Ctrl Pts',(3.43357001355883,59.3237988637257,4.98008002023127));
#7382=CARTESIAN_POINT('Ctrl Pts',(4.59824783273638,59.3423841384353,3.93567293560701));
#7383=CARTESIAN_POINT('Ctrl Pts',(5.07917293181446,59.3523609517956,3.29171663034268));
#7384=CARTESIAN_POINT('Ctrl Pts',(5.7487689124623,59.371817815855,1.88095993765699));
#7385=CARTESIAN_POINT('Ctrl Pts',(5.94166691804369,59.3811237893472,1.13268064497309));
#7386=CARTESIAN_POINT('Ctrl Pts',(6.03738680112009,59.3985674690332,-0.423433560740823));
#7387=CARTESIAN_POINT('Ctrl Pts',(5.92857669505086,59.4073718976364,-1.21710085195043));
#7388=CARTESIAN_POINT('Ctrl Pts',(5.41095745138905,59.4267583370531,-2.70909580482084));
#7389=CARTESIAN_POINT('Ctrl Pts',(5.00996844969224,59.4366766566598,-3.39379981592379));
#7390=CARTESIAN_POINT('Ctrl Pts',(3.98494564711651,59.455591315434,-4.54926395852199));
#7391=CARTESIAN_POINT('Ctrl Pts',(3.37837107878886,59.4640203602861,-5.01619205194707));
#7392=CARTESIAN_POINT('Ctrl Pts',(1.99159585454879,59.4813550505891,-5.71529102862413));
#7393=CARTESIAN_POINT('Ctrl Pts',(1.21827663239224,59.4910215408661,-5.92847273746746));
#7394=CARTESIAN_POINT('Ctrl Pts',(0.283980815507459,59.5027002385771,-5.99496518869567));
#7395=CARTESIAN_POINT('Ctrl Pts',(0.141914105176113,59.5044760724562,-6.));
#7396=CARTESIAN_POINT('Ctrl Pts',(5.58580959264532E-15,59.506249998771,
-6.));
#7397=CARTESIAN_POINT('Origin',(0.,50.,0.));
#7398=CARTESIAN_POINT('',(4.70252513239422E-14,60.0125,-6.));
#7399=CARTESIAN_POINT('',(9.17358507812823E-15,59.956249998771,-6.));
#7400=CARTESIAN_POINT('',(-7.34788079488412E-16,50.,-6.));
#7401=CARTESIAN_POINT('Ctrl Pts',(1.25593979660721E-13,60.0125,-6.));
#7402=CARTESIAN_POINT('Ctrl Pts',(0.141303861427478,60.0107337017321,-6.));
#7403=CARTESIAN_POINT('Ctrl Pts',(0.28275939708923,60.0089655075363,-5.99500839542605));
#7404=CARTESIAN_POINT('Ctrl Pts',(1.21646472782204,59.9972941909021,-5.92884491885588));
#7405=CARTESIAN_POINT('Ctrl Pts',(1.98985001429912,59.9876268748211,-5.71589923330053));
#7406=CARTESIAN_POINT('Ctrl Pts',(3.3768361930805,59.9702895475864,-5.01722489047471));
#7407=CARTESIAN_POINT('Ctrl Pts',(3.98355067371114,59.9618632522133,-4.55048488959786));
#7408=CARTESIAN_POINT('Ctrl Pts',(5.00890949512847,59.9429501315784,-3.3953568347903));
#7409=CARTESIAN_POINT('Ctrl Pts',(5.4101001417314,59.9330321483622,-2.71080031785606));
#7410=CARTESIAN_POINT('Ctrl Pts',(5.92821400384472,59.9136438405904,-1.21891834182566));
#7411=CARTESIAN_POINT('Ctrl Pts',(6.03727302740656,59.9048359031446,-0.425202004778042));
#7412=CARTESIAN_POINT('Ctrl Pts',(5.941984771647,59.8873939952832,1.13099772694377));
#7413=CARTESIAN_POINT('Ctrl Pts',(5.74930537817554,59.878089020869,1.87931094451317));
#7414=CARTESIAN_POINT('Ctrl Pts',(5.08013819823912,59.8586331781096,3.29022086176011));
#7415=CARTESIAN_POINT('Ctrl Pts',(4.59941877272792,59.8486563254349,3.93429954442032));
#7416=CARTESIAN_POINT('Ctrl Pts',(3.43504330283706,59.8300690022009,4.97907042506423));
#7417=CARTESIAN_POINT('Ctrl Pts',(2.76969446582647,59.8221211808227,5.37768131640503));
#7418=CARTESIAN_POINT('Ctrl Pts',(1.31931167178715,59.8039913958972,5.90416531854308));
#7419=CARTESIAN_POINT('Ctrl Pts',(0.547032887913016,59.7943379110988,6.02498930154337));
#7420=CARTESIAN_POINT('Ctrl Pts',(-1.02071810657633,59.7747410236677,5.96567468587889));
#7421=CARTESIAN_POINT('Ctrl Pts',(-1.80078484439692,59.7649901894449,5.77826361325989));
#7422=CARTESIAN_POINT('Ctrl Pts',(-3.21024280951409,59.747371964881,5.12544537310256));
#7423=CARTESIAN_POINT('Ctrl Pts',(-3.83210228483935,59.7391984900125,4.67876614903042));
#7424=CARTESIAN_POINT('Ctrl Pts',(-4.89310404940384,59.7204523559613,3.55964211690044));
#7425=CARTESIAN_POINT('Ctrl Pts',(-5.31551858348093,59.7105756824365,2.89115524293708));
#7426=CARTESIAN_POINT('Ctrl Pts',(-5.88648197201678,59.6909928303025,1.41181471683303));
#7427=CARTESIAN_POINT('Ctrl Pts',(-6.02231852752178,59.6817733575495,0.612810360860394));
#7428=CARTESIAN_POINT('Ctrl Pts',(-5.97294095766319,59.6645217620487,-0.9523156149022));
#7429=CARTESIAN_POINT('Ctrl Pts',(-5.80342604329591,59.6553265314883,-1.70386514775027));
#7430=CARTESIAN_POINT('Ctrl Pts',(-5.17983055745436,59.6359876625287,-3.13028031807604));
#7431=CARTESIAN_POINT('Ctrl Pts',(-4.72104466560709,59.6260115176167,-3.78695695198865));
#7432=CARTESIAN_POINT('Ctrl Pts',(-3.58895685794024,59.6072108315944,-4.87007873323313));
#7433=CARTESIAN_POINT('Ctrl Pts',(-2.93191390328915,59.599148923791,-5.29170631182061));
#7434=CARTESIAN_POINT('Ctrl Pts',(-1.50853114673329,59.5813566393341,-5.85650841985951));
#7435=CARTESIAN_POINT('Ctrl Pts',(-0.757598971356276,59.5719699871419,-5.99999999999999));
#7436=CARTESIAN_POINT('Ctrl Pts',(-5.38458166943201E-14,59.5625,-6.));
#7437=CARTESIAN_POINT('Ctrl Pts',(-1.11022302462516E-14,59.506249998771,
-6.));
#7438=CARTESIAN_POINT('Ctrl Pts',(-0.632821030745593,59.5141602616553,-6.));
#7439=CARTESIAN_POINT('Ctrl Pts',(-1.26260761218587,59.5220325939233,-5.89987618500378));
#7440=CARTESIAN_POINT('Ctrl Pts',(-2.59219414404648,59.5386524255716,-5.46486473433232));
#7441=CARTESIAN_POINT('Ctrl Pts',(-3.26657156372886,59.5465592222212,-5.09055264034919));
#7442=CARTESIAN_POINT('Ctrl Pts',(-4.46476645251953,59.5649116492729,-4.08700619016442));
#7443=CARTESIAN_POINT('Ctrl Pts',(-4.96850192192615,59.5748786230998,-3.45712839551428));
#7444=CARTESIAN_POINT('Ctrl Pts',(-5.68582946429178,59.5944397488744,-2.06429824813703));
#7445=CARTESIAN_POINT('Ctrl Pts',(-5.90313907034519,59.6038529506833,-1.32020767195513));
#7446=CARTESIAN_POINT('Ctrl Pts',(-6.04690002280499,59.6214918266984,0.226201473925191));
#7447=CARTESIAN_POINT('Ctrl Pts',(-5.96548004211257,59.629948119708,1.01450799500909));
#7448=CARTESIAN_POINT('Ctrl Pts',(-5.50263475127271,59.6491224173711,2.51852988851507));
#7449=CARTESIAN_POINT('Ctrl Pts',(-5.12431240893829,59.6590721668368,3.21922386751421));
#7450=CARTESIAN_POINT('Ctrl Pts',(-4.13680068949526,59.6781541992168,4.41180635547012));
#7451=CARTESIAN_POINT('Ctrl Pts',(-3.54553027877212,59.6869308702863,4.89962609971964));
#7452=CARTESIAN_POINT('Ctrl Pts',(-2.18217991660048,59.7039727498135,5.64525560222874));
#7453=CARTESIAN_POINT('Ctrl Pts',(-1.41656447760803,59.7135429428009,5.88422844573759));
#7454=CARTESIAN_POINT('Ctrl Pts',(0.148488043825732,59.7331060993188,6.04859188872487));
#7455=CARTESIAN_POINT('Ctrl Pts',(0.932145238599361,59.7429018142535,5.97817898125281));
#7456=CARTESIAN_POINT('Ctrl Pts',(2.41119858669003,59.7613899811046,5.54668031548456));
#7457=CARTESIAN_POINT('Ctrl Pts',(3.09479081689663,59.7693405589739,5.19632631161659));
#7458=CARTESIAN_POINT('Ctrl Pts',(4.32603853610185,59.7874522861142,4.23409782734767));
#7459=CARTESIAN_POINT('Ctrl Pts',(4.85224268738086,59.7973985542548,3.61910504159258));
#7460=CARTESIAN_POINT('Ctrl Pts',(5.61693867228848,59.8170442900147,2.24580714162143));
#7461=CARTESIAN_POINT('Ctrl Pts',(5.85862805091094,59.8265559336545,1.50669856689779));
#7462=CARTESIAN_POINT('Ctrl Pts',(6.05013056294877,59.8443848385756,-0.0297010951204617));
#7463=CARTESIAN_POINT('Ctrl Pts',(5.99534371003816,59.8525791030305,-0.812909405087863));
#7464=CARTESIAN_POINT('Ctrl Pts',(5.586355194442,59.871535107359,-2.32786044779519));
#7465=CARTESIAN_POINT('Ctrl Pts',(5.23095041176157,59.8815044079573,-3.04359194229456));
#7466=CARTESIAN_POINT('Ctrl Pts',(4.28098368544513,59.9007441194128,-4.27241681121637));
#7467=CARTESIAN_POINT('Ctrl Pts',(3.7044839768511,59.909851938227,-4.78091881232232));
#7468=CARTESIAN_POINT('Ctrl Pts',(2.36423147700459,59.9267863723026,-5.5714596822957));
#7469=CARTESIAN_POINT('Ctrl Pts',(1.60679706958879,59.9361650354012,-5.83515225979701));
#7470=CARTESIAN_POINT('Ctrl Pts',(0.547702715938679,59.9494037148218,-5.98126998655213));
#7471=CARTESIAN_POINT('Ctrl Pts',(0.273718776711667,59.9528285140621,-6.));
#7472=CARTESIAN_POINT('Ctrl Pts',(6.08540995372664E-14,59.956249998771,
-6.));
#7473=CARTESIAN_POINT('Origin',(0.,50.,0.));
#7474=CARTESIAN_POINT('',(3.96941465019781E-15,60.4625,-6.));
#7475=CARTESIAN_POINT('',(-2.9927082070389E-14,60.406249998771,-6.));
#7476=CARTESIAN_POINT('',(-7.34788079488412E-16,50.,-6.));
#7477=CARTESIAN_POINT('Ctrl Pts',(5.44009282066327E-14,60.4625,-6.));
#7478=CARTESIAN_POINT('Ctrl Pts',(0.273148046031432,60.4590856494246,-6.));
#7479=CARTESIAN_POINT('Ctrl Pts',(0.54656143924663,60.4556679820094,-5.98134801383603));
#7480=CARTESIAN_POINT('Ctrl Pts',(1.60512629394782,60.4424359213256,-5.83561176679995));
#7481=CARTESIAN_POINT('Ctrl Pts',(2.36263397232493,60.4330536897797,-5.57213696902889));
#7482=CARTESIAN_POINT('Ctrl Pts',(3.70309278914091,60.4161222630287,-4.78199302095628));
#7483=CARTESIAN_POINT('Ctrl Pts',(4.2797245897032,60.407015601891,-4.27367422475566));
#7484=CARTESIAN_POINT('Ctrl Pts',(5.23002905006472,60.3877772352197,-3.04516857252226));
#7485=CARTESIAN_POINT('Ctrl Pts',(5.58564006177245,60.3778080583442,-2.32956757343556));
#7486=CARTESIAN_POINT('Ctrl Pts',(5.99510697394861,60.3588500744187,-0.814709865771511));
#7487=CARTESIAN_POINT('Ctrl Pts',(6.05012927819066,60.3506538419049,-0.0314571757089235));
#7488=CARTESIAN_POINT('Ctrl Pts',(5.85905319689185,60.3328266168241,1.5050335092036));
#7489=CARTESIAN_POINT('Ctrl Pts',(5.61758195090551,60.3233158153094,2.2441902306893));
#7490=CARTESIAN_POINT('Ctrl Pts',(4.85330844088509,60.3036707493072,3.61767017708307));
#7491=CARTESIAN_POINT('Ctrl Pts',(4.32730392870041,60.293724247221,4.23279983549354));
#7492=CARTESIAN_POINT('Ctrl Pts',(3.09635036143289,60.2756103299423,5.19540046477978));
#7493=CARTESIAN_POINT('Ctrl Pts',(2.41284204109846,60.2676605255137,5.54596868127766));
#7494=CARTESIAN_POINT('Ctrl Pts',(0.933915368168958,60.2491739421021,5.97789972053624));
#7495=CARTESIAN_POINT('Ctrl Pts',(0.1503026571044,60.2393787832138,6.04854411681298));
#7496=CARTESIAN_POINT('Ctrl Pts',(-1.41477809332879,60.2198152738334,5.88465836872042));
#7497=CARTESIAN_POINT('Ctrl Pts',(-2.18046716029772,60.2102441604963,5.64591753364946));
#7498=CARTESIAN_POINT('Ctrl Pts',(-3.54403161793187,60.1931996047758,4.90070794687794));
#7499=CARTESIAN_POINT('Ctrl Pts',(-4.13543995211808,60.1844264853552,4.41307932512849));
#7500=CARTESIAN_POINT('Ctrl Pts',(-5.12329644157916,60.1653459517617,3.2208343421969));
#7501=CARTESIAN_POINT('Ctrl Pts',(-5.50182840474064,60.1553964364731,2.52028302020345));
#7502=CARTESIAN_POINT('Ctrl Pts',(-5.96517307028057,60.1362201587863,1.01636653405098));
#7503=CARTESIAN_POINT('Ctrl Pts',(-6.04684129149082,60.1277610588246,0.228011856647941));
#7504=CARTESIAN_POINT('Ctrl Pts',(-5.90352058767477,60.1101239535066,-1.31848789690941));
#7505=CARTESIAN_POINT('Ctrl Pts',(-5.68643532461062,60.100711697856,-2.0626205952178));
#7506=CARTESIAN_POINT('Ctrl Pts',(-4.96954506868888,60.0811514416167,-3.4556228858106));
#7507=CARTESIAN_POINT('Ctrl Pts',(-4.4660178099647,60.071184327976,-4.08563380639988));
#7508=CARTESIAN_POINT('Ctrl Pts',(-3.26812887880239,60.0528297240221,-5.08955799492021));
#7509=CARTESIAN_POINT('Ctrl Pts',(-2.59383484350845,60.0449229355437,-5.46409084992291));
#7510=CARTESIAN_POINT('Ctrl Pts',(-1.26378368350271,60.0282972960437,-5.89968791431417));
#7511=CARTESIAN_POINT('Ctrl Pts',(-0.633415724091756,60.0204176965511,-6.));
#7512=CARTESIAN_POINT('Ctrl Pts',(1.23512311489549E-13,60.0125,-6.));
#7513=CARTESIAN_POINT('Ctrl Pts',(6.39766017940246E-14,59.956249998771,
-6.));
#7514=CARTESIAN_POINT('Ctrl Pts',(-0.504816217535487,59.9625602014901,-6.));
#7515=CARTESIAN_POINT('Ctrl Pts',(-1.008730511896,59.9688591301697,-5.93628708717274));
#7516=CARTESIAN_POINT('Ctrl Pts',(-2.23495289718686,59.9841869099859,-5.61976064930326));
#7517=CARTESIAN_POINT('Ctrl Pts',(-2.92758705550944,59.9922591355636,-5.2920648335774));
#7518=CARTESIAN_POINT('Ctrl Pts',(-4.18209374514919,60.0100264655069,-4.37507897245537));
#7519=CARTESIAN_POINT('Ctrl Pts',(-4.72403710285573,60.0198179136244,-3.78347488288704));
#7520=CARTESIAN_POINT('Ctrl Pts',(-5.53488436650716,60.0394089485369,-2.44187548395896));
#7521=CARTESIAN_POINT('Ctrl Pts',(-5.80315545641587,60.0490179289523,-1.70912228121668));
#7522=CARTESIAN_POINT('Ctrl Pts',(-6.0465703131164,60.067048945809,-0.184023924503232));
#7523=CARTESIAN_POINT('Ctrl Pts',(-6.0201409300119,60.0750538718755,0.593955224774895));
#7524=CARTESIAN_POINT('Ctrl Pts',(-5.66901998337537,60.0937652990181,2.11972305133975));
#7525=CARTESIAN_POINT('Ctrl Pts',(-5.33889794584649,60.1037429188537,2.85082004378456));
#7526=CARTESIAN_POINT('Ctrl Pts',(-4.4305494316801,60.1231333270827,4.11759397032116));
#7527=CARTESIAN_POINT('Ctrl Pts',(-3.87044926128686,60.1323758654756,4.64800911083874));
#7528=CARTESIAN_POINT('Ctrl Pts',(-2.552659102628,60.149708509365,5.48830366644853));
#7529=CARTESIAN_POINT('Ctrl Pts',(-1.80044317137907,60.1587444591288,5.7789253132565));
#7530=CARTESIAN_POINT('Ctrl Pts',(-0.240323360944891,60.1782459567593,6.04627958233635));
#7531=CARTESIAN_POINT('Ctrl Pts',(0.551317277502825,60.1881414647399,6.02588609015704));
#7532=CARTESIAN_POINT('Ctrl Pts',(2.05673048868537,60.2069591298796,5.68730090375562));
#7533=CARTESIAN_POINT('Ctrl Pts',(2.75862633972365,60.2152299829837,5.38196040493909));
#7534=CARTESIAN_POINT('Ctrl Pts',(4.04091497351422,60.2327291587413,4.50578547936514));
#7535=CARTESIAN_POINT('Ctrl Pts',(4.60133380314792,60.2424456885497,3.93176886543798));
#7536=CARTESIAN_POINT('Ctrl Pts',(5.45569031524612,60.26204279983,2.61472823199752));
#7537=CARTESIAN_POINT('Ctrl Pts',(5.74761730637461,60.2717294731965,1.88845580279189));
#7538=CARTESIAN_POINT('Ctrl Pts',(6.03721775271674,60.2899362502433,0.373786677800705));
#7539=CARTESIAN_POINT('Ctrl Pts',(6.03554735569943,60.2978563703102,-0.399853629555168));
#7540=CARTESIAN_POINT('Ctrl Pts',(5.73527461721579,60.3163448718056,-1.93438569360858));
#7541=CARTESIAN_POINT('Ctrl Pts',(5.42789447758374,60.326318871908,-2.67827835028817));
#7542=CARTESIAN_POINT('Ctrl Pts',(4.55732677402955,60.3458218758435,-3.97726618384324));
#7543=CARTESIAN_POINT('Ctrl Pts',(4.01231068105578,60.3551739173839,-4.52650558797703));
#7544=CARTESIAN_POINT('Ctrl Pts',(2.726135453839,60.3727001821279,-5.4029389611706));
#7545=CARTESIAN_POINT('Ctrl Pts',(1.99216620776156,60.381347921174,-5.71444259303174));
#7546=CARTESIAN_POINT('Ctrl Pts',(0.817020770296382,60.3960372391423,-5.95827073896467));
#7547=CARTESIAN_POINT('Ctrl Pts',(0.408553452683297,60.4011430806124,-6.));
#7548=CARTESIAN_POINT('Ctrl Pts',(4.71844785465692E-15,60.406249998771,
-6.));
#7549=CARTESIAN_POINT('Origin',(0.,50.,0.));
#7550=CARTESIAN_POINT('',(-3.71478685391425E-14,60.9125,-6.));
#7551=CARTESIAN_POINT('',(4.03880358923688E-15,60.856249998771,-6.));
#7552=CARTESIAN_POINT('',(-7.34788079488412E-16,50.,-6.));
#7553=CARTESIAN_POINT('Ctrl Pts',(-1.12618248060414E-13,60.9125,-5.99999999999999));
#7554=CARTESIAN_POINT('Ctrl Pts',(0.407899687187211,60.9074012539101,-6.));
#7555=CARTESIAN_POINT('Ctrl Pts',(0.815716773773336,60.9023035403277,-5.95840419235766));
#7556=CARTESIAN_POINT('Ctrl Pts',(1.99037501211202,60.8876203123485,-5.71507748822328));
#7557=CARTESIAN_POINT('Ctrl Pts',(2.72451380599383,60.8789692960728,-5.40376825943217));
#7558=CARTESIAN_POINT('Ctrl Pts',(4.0109879068283,60.8614448350747,-4.52767406390134));
#7559=CARTESIAN_POINT('Ctrl Pts',(4.55614945694963,60.8520937890426,-3.97861060060485));
#7560=CARTESIAN_POINT('Ctrl Pts',(5.4270793932076,60.8325917617613,-2.67992212165016));
#7561=CARTESIAN_POINT('Ctrl Pts',(5.73467668753441,60.8226176794372,-1.93614724397326));
#7562=CARTESIAN_POINT('Ctrl Pts',(6.0354300753238,60.8041270371724,-0.401694927124871));
#7563=CARTESIAN_POINT('Ctrl Pts',(6.03733400582058,60.7962064800698,0.371985158761497));
#7564=CARTESIAN_POINT('Ctrl Pts',(5.74817275039893,60.7780013559698,1.88675515806456));
#7565=CARTESIAN_POINT('Ctrl Pts',(5.45647056996206,60.7683153808155,2.61309288370565));
#7566=CARTESIAN_POINT('Ctrl Pts',(4.60252525073201,60.7487182333133,3.93037426549416));
#7567=CARTESIAN_POINT('Ctrl Pts',(4.04227975119642,60.7390009421187,4.50456128543735));
#7568=CARTESIAN_POINT('Ctrl Pts',(2.76025366510501,60.721499184061,5.38112633567564));
#7569=CARTESIAN_POINT('Ctrl Pts',(2.05844775600324,60.71323059695,5.68667991738853));
#7570=CARTESIAN_POINT('Ctrl Pts',(0.55315772214554,60.6944144715268,6.0257142941801));
#7571=CARTESIAN_POINT('Ctrl Pts',(-0.238451892510666,60.6845193513435,6.04635055945311));
#7572=CARTESIAN_POINT('Ctrl Pts',(-1.79871426147577,60.6650160717315,5.77947524572385));
#7573=CARTESIAN_POINT('Ctrl Pts',(-2.55109564768498,60.6559762829156,5.48904274206938));
#7574=CARTESIAN_POINT('Ctrl Pts',(-3.86916759984809,60.6386453907715,4.64907269931894));
#7575=CARTESIAN_POINT('Ctrl Pts',(-4.42939943296648,60.6294038661924,4.11882722641972));
#7576=CARTESIAN_POINT('Ctrl Pts',(-5.33807972820677,60.6100145454816,2.85234531440023));
#7577=CARTESIAN_POINT('Ctrl Pts',(-5.66840233303937,60.6000369394427,2.12136539403535));
#7578=CARTESIAN_POINT('Ctrl Pts',(-6.01997653921377,60.5813235580555,0.595678731588266));
#7579=CARTESIAN_POINT('Ctrl Pts',(-6.04662719473821,60.5733175290641,-0.1823402310685));
#7580=CARTESIAN_POINT('Ctrl Pts',(-5.80362157445076,60.5552880868231,-1.70752940377283));
#7581=CARTESIAN_POINT('Ctrl Pts',(-5.53556014903915,60.545679832871,-2.44033654855703));
#7582=CARTESIAN_POINT('Ctrl Pts',(-4.72510067103932,60.5260889405219,-3.7821466661943));
#7583=CARTESIAN_POINT('Ctrl Pts',(-4.18332318495113,60.5162968750893,-4.37390354690658));
#7584=CARTESIAN_POINT('Ctrl Pts',(-2.92906424335277,60.4985272003166,-5.29124905149095));
#7585=CARTESIAN_POINT('Ctrl Pts',(-2.23651043720591,60.490456380465,-5.61914254328846));
#7586=CARTESIAN_POINT('Ctrl Pts',(-1.00982889950544,60.4751228612438,-5.93614756202184));
#7587=CARTESIAN_POINT('Ctrl Pts',(-0.505368605494469,60.4688171075687,-6.));
#7588=CARTESIAN_POINT('Ctrl Pts',(6.12010442324618E-14,60.4625,-6.));
#7589=CARTESIAN_POINT('Ctrl Pts',(1.02001740387436E-14,60.406249998771,
-6.));
#7590=CARTESIAN_POINT('Ctrl Pts',(-0.374775140832848,60.4109346880314,-6.));
#7591=CARTESIAN_POINT('Ctrl Pts',(-0.749622762601871,60.4156202833035,-5.96488608497845));
#7592=CARTESIAN_POINT('Ctrl Pts',(-1.8652081247458,60.4295651003303,-5.75300152969955));
#7593=CARTESIAN_POINT('Ctrl Pts',(-2.57723487707561,60.4381304044621,-5.47118475110046));
#7594=CARTESIAN_POINT('Ctrl Pts',(-3.88822754079226,60.4553417616544,-4.63816964510487));
#7595=CARTESIAN_POINT('Ctrl Pts',(-4.46742436471921,60.464968789911,-4.08326231043965));
#7596=CARTESIAN_POINT('Ctrl Pts',(-5.36668868053248,60.4845507847614,-2.79354560554172));
#7597=CARTESIAN_POINT('Ctrl Pts',(-5.68331709127291,60.4943094131409,-2.07488762823363));
#7598=CARTESIAN_POINT('Ctrl Pts',(-6.02124370086058,60.5126958643704,-0.571522036550122));
#7599=CARTESIAN_POINT('Ctrl Pts',(-6.04506729549864,60.520610878074,0.19792028182648));
#7600=CARTESIAN_POINT('Ctrl Pts',(-5.79733980704217,60.5388616662783,1.74083034691086));
#7601=CARTESIAN_POINT('Ctrl Pts',(-5.51393640302953,60.5488211493281,2.49722495048716));
#7602=CARTESIAN_POINT('Ctrl Pts',(-4.68353189440874,60.5684207561163,3.82832480471795));
#7603=CARTESIAN_POINT('Ctrl Pts',(-4.15473832948569,60.5778770003157,4.39655611911274));
#7604=CARTESIAN_POINT('Ctrl Pts',(-2.90124178378718,60.5955974837708,5.30979769390625));
#7605=CARTESIAN_POINT('Ctrl Pts',(-2.18546918107772,60.6039316340075,5.64224146324259));
#7606=CARTESIAN_POINT('Ctrl Pts',(-0.658912830584277,60.6230135883887,6.01578392027695));
#7607=CARTESIAN_POINT('Ctrl Pts',(0.13784785586468,60.6329730969693,6.05019149924373));
#7608=CARTESIAN_POINT('Ctrl Pts',(1.66990313276243,60.6521237879305,5.81289815367829));
#7609=CARTESIAN_POINT('Ctrl Pts',(2.39249044702777,60.6610720459385,5.554665520313));
#7610=CARTESIAN_POINT('Ctrl Pts',(3.73167477624232,60.6779902018836,4.76501165102443));
#7611=CARTESIAN_POINT('Ctrl Pts',(4.32893078259873,60.6875170653545,4.22978361675552));
#7612=CARTESIAN_POINT('Ctrl Pts',(5.27210873015133,60.7070620082945,2.96884316782837));
#7613=CARTESIAN_POINT('Ctrl Pts',(5.61319037689518,60.7168824116893,2.25859674143006));
#7614=CARTESIAN_POINT('Ctrl Pts',(5.99916745926047,60.7354430011218,0.766886905010639));
#7615=CARTESIAN_POINT('Ctrl Pts',(6.04798468727948,60.7434365357459,0.00125250179310366));
#7616=CARTESIAN_POINT('Ctrl Pts',(5.85182540957717,60.7614472214852,-1.54925076800202));
#7617=CARTESIAN_POINT('Ctrl Pts',(5.59237936868007,60.7713818229691,-2.31717870101808));
#7618=CARTESIAN_POINT('Ctrl Pts',(4.80242486574243,60.7910565371578,-3.67857050139044));
#7619=CARTESIAN_POINT('Ctrl Pts',(4.29014923672744,60.8006060031449,-4.26494991040273));
#7620=CARTESIAN_POINT('Ctrl Pts',(3.06873797490042,60.818511480103,-5.21380490027025));
#7621=CARTESIAN_POINT('Ctrl Pts',(2.37017279154696,60.8266228388767,-5.56625543273656));
#7622=CARTESIAN_POINT('Ctrl Pts',(1.09432066564828,60.8425709904504,-5.92495590370132));
#7623=CARTESIAN_POINT('Ctrl Pts',(0.547865501629616,60.8494016800006,-6.));
#7624=CARTESIAN_POINT('Ctrl Pts',(-6.10622663543836E-14,60.8562499987709,
-6.));
#7625=CARTESIAN_POINT('Origin',(0.,50.,0.));
#7626=CARTESIAN_POINT('',(-4.89396513670948E-14,61.3625,-6.));
#7627=CARTESIAN_POINT('',(-1.48002933598712E-14,61.306249998771,-6.));
#7628=CARTESIAN_POINT('',(-7.34788079488412E-16,50.,-6.));
#7629=CARTESIAN_POINT('Ctrl Pts',(-5.87030424270552E-14,61.3625,-6.));
#7630=CARTESIAN_POINT('Ctrl Pts',(0.547256010313519,61.3556592998711,-6.));
#7631=CARTESIAN_POINT('Ctrl Pts',(1.09311032710014,61.3488361209112,-5.92512279942422));
#7632=CARTESIAN_POINT('Ctrl Pts',(2.36853671641672,61.3328932910448,-5.5669593249633));
#7633=CARTESIAN_POINT('Ctrl Pts',(3.0672535886464,61.3247803003645,-5.21468631722413));
#7634=CARTESIAN_POINT('Ctrl Pts',(4.28895308880416,61.3068764604378,-4.26614896431677));
#7635=CARTESIAN_POINT('Ctrl Pts',(4.80137959754346,61.2973277913116,-3.67993027661039));
#7636=CARTESIAN_POINT('Ctrl Pts',(5.59170169867098,61.2776536644745,-2.3188049663686));
#7637=CARTESIAN_POINT('Ctrl Pts',(5.85136464186537,61.2677187928075,-1.55097730351244));
#7638=CARTESIAN_POINT('Ctrl Pts',(6.04798705243048,61.2497059219882,-0.000539574551999683));
#7639=CARTESIAN_POINT('Ctrl Pts',(5.99939436944144,61.2417134657263,0.765127586001477));
#7640=CARTESIAN_POINT('Ctrl Pts',(5.61385165226514,61.2231544295715,2.25694471763481));
#7641=CARTESIAN_POINT('Ctrl Pts',(5.27299041396996,61.2133345401954,2.96727091390557));
#7642=CARTESIAN_POINT('Ctrl Pts',(4.33020581697961,61.1937891634826,4.22847853409));
#7643=CARTESIAN_POINT('Ctrl Pts',(3.73311018750954,61.1842613450504,4.76388737754585));
#7644=CARTESIAN_POINT('Ctrl Pts',(2.39417921764515,61.1673405080427,5.55393518987752));
#7645=CARTESIAN_POINT('Ctrl Pts',(1.67168965651797,61.1583961207065,5.81238209134706));
#7646=CARTESIAN_POINT('Ctrl Pts',(0.139752350124207,61.1392469043765,6.05014450555849));
#7647=CARTESIAN_POINT('Ctrl Pts',(-0.656993188943331,61.1292875851381,6.01599054763202));
#7648=CARTESIAN_POINT('Ctrl Pts',(-2.1837109481026,61.1102036131486,5.64293150348842));
#7649=CARTESIAN_POINT('Ctrl Pts',(-2.89964817697339,61.10186697484,5.31067801891126));
#7650=CARTESIAN_POINT('Ctrl Pts',(-4.15344592677298,61.0841482546054,4.39777322371879));
#7651=CARTESIAN_POINT('Ctrl Pts',(-4.68239184360215,61.074692928492,3.82971467889929));
#7652=CARTESIAN_POINT('Ctrl Pts',(-5.51317144959492,61.0550941196616,2.49890509940508));
#7653=CARTESIAN_POINT('Ctrl Pts',(-5.79679788338461,61.0451344528347,1.7426222855376));
#7654=CARTESIAN_POINT('Ctrl Pts',(-6.04500959707094,61.0268814413336,0.199786408658281));
#7655=CARTESIAN_POINT('Ctrl Pts',(-6.02142071315293,61.0189667699931,-0.569693169468934));
#7656=CARTESIAN_POINT('Ctrl Pts',(-5.68394232834918,61.0005819647083,-2.07316549798162));
#7657=CARTESIAN_POINT('Ctrl Pts',(-5.36754261280559,60.9908239588702,-2.79189800462317));
#7658=CARTESIAN_POINT('Ctrl Pts',(-4.46869156830285,60.971241722063,-4.08187566283363));
#7659=CARTESIAN_POINT('Ctrl Pts',(-3.88966615171452,60.9616138117079,-4.63696344433425));
#7660=CARTESIAN_POINT('Ctrl Pts',(-2.57893806597757,60.9443997520077,-5.47038095148736));
#7661=CARTESIAN_POINT('Ctrl Pts',(-1.8670074758115,60.9358375934475,-5.75241671135876));
#7662=CARTESIAN_POINT('Ctrl Pts',(-0.750876861534743,60.9218859607691,-5.9647682424307));
#7663=CARTESIAN_POINT('Ctrl Pts',(-0.37540344890043,60.9171925431112,-5.99999999999999));
#7664=CARTESIAN_POINT('Ctrl Pts',(-1.36834987785051E-13,60.9125,-6.));
#7665=CARTESIAN_POINT('Ctrl Pts',(-6.57113252700015E-14,60.856249998771,
-6.));
#7666=CARTESIAN_POINT('Ctrl Pts',(-0.241384366345414,60.8592673033503,-6.));
#7667=CARTESIAN_POINT('Ctrl Pts',(-0.483042507482243,60.8622880301145,-5.98543381416668));
#7668=CARTESIAN_POINT('Ctrl Pts',(-1.48088634413119,60.8747610780727,-5.86420003251657));
#7669=CARTESIAN_POINT('Ctrl Pts',(-2.21368102725674,60.8839210116117,-5.62863230028752));
#7670=CARTESIAN_POINT('Ctrl Pts',(-3.57931748887809,60.900991467382,-4.8805142091203));
#7671=CARTESIAN_POINT('Ctrl Pts',(-4.19329126295089,60.9102129319999,-4.36431882558091));
#7672=CARTESIAN_POINT('Ctrl Pts',(-5.17736054272197,60.9297063369937,-3.13174786985753));
#7673=CARTESIAN_POINT('Ctrl Pts',(-5.54138977875599,60.9395759150596,-2.43020767878148));
#7674=CARTESIAN_POINT('Ctrl Pts',(-5.97274844708689,60.9582966042501,-0.949909531091851));
#7675=CARTESIAN_POINT('Ctrl Pts',(-6.04490483620197,60.9664392786842,-0.187529359001643));
#7676=CARTESIAN_POINT('Ctrl Pts',(-5.89783656108435,60.9840994066076,1.35893347045698));
#7677=CARTESIAN_POINT('Ctrl Pts',(-5.66628129051843,60.9938619224954,2.127067560783));
#7678=CARTESIAN_POINT('Ctrl Pts',(-4.92705043276294,61.0134577989134,3.51046195006189));
#7679=CARTESIAN_POINT('Ctrl Pts',(-4.43354966296899,61.0230991102351,4.11616533768471));
#7680=CARTESIAN_POINT('Ctrl Pts',(-3.24738852655604,61.0412014054,5.10355328409652));
#7681=CARTESIAN_POINT('Ctrl Pts',(-2.56698280158148,61.0491627137512,5.47744365620462));
#7682=CARTESIAN_POINT('Ctrl Pts',(-1.07720954505616,61.0677848794577,5.95586496370465));
#7683=CARTESIAN_POINT('Ctrl Pts',(-0.279018307134967,61.0777622699318,6.04606057744179));
#7684=CARTESIAN_POINT('Ctrl Pts',(1.27603635701102,61.0972004532336,5.91248695432248));
#7685=CARTESIAN_POINT('Ctrl Pts',(2.01906250364592,61.1064882800665,5.70168173011325));
#7686=CARTESIAN_POINT('Ctrl Pts',(3.41199186546582,61.1238998970893,4.99899641261455));
#7687=CARTESIAN_POINT('Ctrl Pts',(4.04343943853173,61.1327687624584,4.50358454524063));
#7688=CARTESIAN_POINT('Ctrl Pts',(5.07048391380239,61.1521888498299,3.30259812204962));
#7689=CARTESIAN_POINT('Ctrl Pts',(5.45882490112482,61.1621009426495,2.6111669823951));
#7690=CARTESIAN_POINT('Ctrl Pts',(5.93867573146569,61.1809877182057,1.14352339622535));
#7691=CARTESIAN_POINT('Ctrl Pts',(6.03554840659564,61.1893681387995,0.384255003332309));
#7692=CARTESIAN_POINT('Ctrl Pts',(5.93903175788826,61.2067504862316,-1.16573355860694));
#7693=CARTESIAN_POINT('Ctrl Pts',(5.73269741445749,61.2164317837732,-1.9409263285586));
#7694=CARTESIAN_POINT('Ctrl Pts',(5.03801375396834,61.2360253839997,-3.34982978860118));
#7695=CARTESIAN_POINT('Ctrl Pts',(4.56267011496105,61.2457426558097,-3.97303312990549));
#7696=CARTESIAN_POINT('Ctrl Pts',(3.40957040924791,61.2640234453728,-4.99599770845838));
#7697=CARTESIAN_POINT('Ctrl Pts',(2.74550424329715,61.2719311957298,-5.38956113336518));
#7698=CARTESIAN_POINT('Ctrl Pts',(1.37485673432524,61.2890642895919,-5.88111192017016));
#7699=CARTESIAN_POINT('Ctrl Pts',(0.689573200401228,61.2976303337659,-6.));
#7700=CARTESIAN_POINT('Ctrl Pts',(7.07767178198537E-15,61.306249998771,
-6.));
#7701=CARTESIAN_POINT('Origin',(0.,50.,0.));
#7702=CARTESIAN_POINT('',(-7.34788079488412E-16,73.,-6.));
#7703=CARTESIAN_POINT('Origin',(0.,73.,0.));
#7704=CARTESIAN_POINT('',(-1.33431256400507E-14,62.206249998771,-6.));
#7705=CARTESIAN_POINT('',(-7.34788079488412E-16,50.,-6.));
#7706=CARTESIAN_POINT('',(-3.,62.393749998771,5.19615242270663));
#7707=CARTESIAN_POINT('Ctrl Pts',(-8.60422844084496E-15,62.206249998771,
-6.));
#7708=CARTESIAN_POINT('Ctrl Pts',(-0.616258639618391,62.2139532317662,-6.));
#7709=CARTESIAN_POINT('Ctrl Pts',(-1.22983984371762,62.2216229968174,-5.90504861391718));
#7710=CARTESIAN_POINT('Ctrl Pts',(-2.5464240496641,62.2380802993918,-5.48621753855818));
#7711=CARTESIAN_POINT('Ctrl Pts',(-3.22312814105713,62.2459901750686,-5.11803689285341));
#7712=CARTESIAN_POINT('Ctrl Pts',(-4.42981084459672,62.2642818352613,-4.12500428678142));
#7713=CARTESIAN_POINT('Ctrl Pts',(-4.93932139761823,62.2742445554702,-3.49885367060309));
#7714=CARTESIAN_POINT('Ctrl Pts',(-5.66878983733698,62.2938291823633,-2.11086213324869));
#7715=CARTESIAN_POINT('Ctrl Pts',(-5.89233336963267,62.3032683826333,-1.36796908110026));
#7716=CARTESIAN_POINT('Ctrl Pts',(-6.04832001623241,62.320956297192,0.175911543593013));
#7717=CARTESIAN_POINT('Ctrl Pts',(-5.97377394326822,62.3293374875246,0.962888696203115));
#7718=CARTESIAN_POINT('Ctrl Pts',(-5.53012411876458,62.348228845472,2.45185624599821));
#7719=CARTESIAN_POINT('Ctrl Pts',(-5.16982972712595,62.3579423477225,3.14113508425838));
#7720=CARTESIAN_POINT('Ctrl Pts',(-4.22166673971517,62.3767254531342,4.32882188275267));
#7721=CARTESIAN_POINT('Ctrl Pts',(-3.64876120915662,62.3856404836565,4.82158996396027));
#7722=CARTESIAN_POINT('Ctrl Pts',(-3.,62.393749998771,5.19615242270663));
#7723=CARTESIAN_POINT('',(-3.,62.,5.19615242270663));
#7724=CARTESIAN_POINT('',(-3.,50.,5.19615242270663));
#7725=CARTESIAN_POINT('',(-2.54168010328493E-14,61.8125,-6.));
#7726=CARTESIAN_POINT('Ctrl Pts',(-3.,62.,5.19615242270663));
#7727=CARTESIAN_POINT('Ctrl Pts',(-3.53098416040067,61.993362697995,4.88958857476387));
#7728=CARTESIAN_POINT('Ctrl Pts',(-4.01184980938664,61.986177110606,4.50344035651509));
#7729=CARTESIAN_POINT('Ctrl Pts',(-4.85405966080593,61.9709529731779,3.58334486618095));
#7730=CARTESIAN_POINT('Ctrl Pts',(-5.20541786447774,61.9629893514596,3.0505537568201));
#7731=CARTESIAN_POINT('Ctrl Pts',(-5.79411617403706,61.9452204120402,1.7490145711897));
#7732=CARTESIAN_POINT('Ctrl Pts',(-5.97451271881476,61.9356327682269,0.96749796704209));
#7733=CARTESIAN_POINT('Ctrl Pts',(-6.01945738911264,61.9185397802293,-0.585535810928422));
#7734=CARTESIAN_POINT('Ctrl Pts',(-5.89710840746593,61.9098297568449,-1.34196254642815));
#7735=CARTESIAN_POINT('Ctrl Pts',(-5.36693302400083,61.8907764468428,-2.79593503145085));
#7736=CARTESIAN_POINT('Ctrl Pts',(-4.95364215667331,61.8808313385913,-3.47601118612493));
#7737=CARTESIAN_POINT('Ctrl Pts',(-3.88906935822695,61.8616193564059,-4.63610668819626));
#7738=CARTESIAN_POINT('Ctrl Pts',(-3.24866047005788,61.8531082558757,-5.10534405456059));
#7739=CARTESIAN_POINT('Ctrl Pts',(-1.84025893941671,61.8355032367427,-5.76218771758364));
#7740=CARTESIAN_POINT('Ctrl Pts',(-1.08865709430635,61.8261082136788,-5.95014037299404));
#7741=CARTESIAN_POINT('Ctrl Pts',(-0.214690057248332,61.8151836257155,-5.99712208047878));
#7742=CARTESIAN_POINT('Ctrl Pts',(-0.107293209532287,61.8138411651192,-6.));
#7743=CARTESIAN_POINT('Ctrl Pts',(-1.49186218934005E-15,61.8125,-6.));
#7744=CARTESIAN_POINT('',(3.0510683832643E-14,61.756249998771,-6.));
#7745=CARTESIAN_POINT('',(-7.34788079488412E-16,50.,-6.));
#7746=CARTESIAN_POINT('Ctrl Pts',(6.59194920871187E-14,61.756249998771,
-6.));
#7747=CARTESIAN_POINT('Ctrl Pts',(-0.742391456204802,61.7655298919735,-6.));
#7748=CARTESIAN_POINT('Ctrl Pts',(-1.47865620397113,61.7747332013206,-5.86220905952843));
#7749=CARTESIAN_POINT('Ctrl Pts',(-2.89102875013166,61.7923878581476,-5.31395788022286));
#7750=CARTESIAN_POINT('Ctrl Pts',(-3.55017353252816,61.8004138992099,-4.89821050585146));
#7751=CARTESIAN_POINT('Ctrl Pts',(-4.69053249859411,61.819160949478,-3.8248187388743));
#7752=CARTESIAN_POINT('Ctrl Pts',(-5.15493007592081,61.8291381888529,-3.17128091093427));
#7753=CARTESIAN_POINT('Ctrl Pts',(-5.79015585618769,61.848508488155,-1.74867708355258));
#7754=CARTESIAN_POINT('Ctrl Pts',(-5.96556963804746,61.857732393193,-0.997884428661905));
#7755=CARTESIAN_POINT('Ctrl Pts',(-6.02667359503539,61.8750329475164,0.564993936637363));
#7756=CARTESIAN_POINT('Ctrl Pts',(-5.89773406647016,61.8841401236578,1.36263557514336));
#7757=CARTESIAN_POINT('Ctrl Pts',(-5.3403131920318,61.9036740996705,2.84527989272617));
#7758=CARTESIAN_POINT('Ctrl Pts',(-4.92327593914152,61.9135623679774,3.51794242151836));
#7759=CARTESIAN_POINT('Ctrl Pts',(-3.87135978464613,61.9323517826686,4.64631012732954));
#7760=CARTESIAN_POINT('Ctrl Pts',(-3.25341935648662,61.9405822568149,5.09812450710615));
#7761=CARTESIAN_POINT('Ctrl Pts',(-1.84970608968904,61.9581286726499,5.76278650867087));
#7762=CARTESIAN_POINT('Ctrl Pts',(-1.0712790534765,61.9678590106026,5.9567999023865));
#7763=CARTESIAN_POINT('Ctrl Pts',(0.496519932524449,61.9874564979276,6.0294433272045));
#7764=CARTESIAN_POINT('Ctrl Pts',(1.27041985657347,61.9971302469782,5.91496086919199));
#7765=CARTESIAN_POINT('Ctrl Pts',(2.72453340113302,62.0153066662852,5.40053328082097));
#7766=CARTESIAN_POINT('Ctrl Pts',(3.39218254958916,62.0232359218829,5.0081872966928));
#7767=CARTESIAN_POINT('Ctrl Pts',(4.56530468786986,62.041763606212,3.97397551344385));
#7768=CARTESIAN_POINT('Ctrl Pts',(5.05197530023428,62.0517389691394,3.33347036706901));
#7769=CARTESIAN_POINT('Ctrl Pts',(5.73356113214312,62.0712237843013,1.92705400599191));
#7770=CARTESIAN_POINT('Ctrl Pts',(5.93257678186554,62.0805574372898,1.17974981446382));
#7771=CARTESIAN_POINT('Ctrl Pts',(6.04036429280152,62.0980505239439,-0.373961163281768));
#7772=CARTESIAN_POINT('Ctrl Pts',(5.93849275700343,62.1067595872934,-1.1662630863717));
#7773=CARTESIAN_POINT('Ctrl Pts',(5.43468465290227,62.1260935095028,-2.66138057257977));
#7774=CARTESIAN_POINT('Ctrl Pts',(5.03934834315488,62.136020843486,-3.35018087933003));
#7775=CARTESIAN_POINT('Ctrl Pts',(4.02372723450545,62.1549782617169,-4.51502304185605));
#7776=CARTESIAN_POINT('Ctrl Pts',(3.42104652316216,62.1634869172315,-4.98720673948494));
#7777=CARTESIAN_POINT('Ctrl Pts',(2.04016613534585,62.1807479220792,-5.69812985528455));
#7778=CARTESIAN_POINT('Ctrl Pts',(1.26871736126363,62.1903910317553,-5.9178795864489));
#7779=CARTESIAN_POINT('Ctrl Pts',(0.318012786659299,62.2022748389378,-5.99368644877733));
#7780=CARTESIAN_POINT('Ctrl Pts',(0.158917369613548,62.2042635316508,-6.));
#7781=CARTESIAN_POINT('Ctrl Pts',(3.85108611666851E-15,62.206249998771,
-6.));
#7782=CARTESIAN_POINT('Origin',(-32.5,400.,0.));
#7783=CARTESIAN_POINT('',(-59.,400.,-7.34788079488412E-16));
#7784=CARTESIAN_POINT('Origin',(-65.,400.,0.));
#7785=CARTESIAN_POINT('',(-6.,400.,-7.34788079488412E-16));
#7786=CARTESIAN_POINT('Origin',(-32.5,400.,-7.34788079488412E-16));
#7787=CARTESIAN_POINT('',(-7.34788079488412E-16,400.,-6.));
#7788=CARTESIAN_POINT('Origin',(0.,400.,0.));
#7789=CARTESIAN_POINT('Origin',(0.,400.,0.));
#7790=CARTESIAN_POINT('Origin',(0.,50.,0.));
#7791=CARTESIAN_POINT('Ctrl Pts',(6.10622663543836E-15,61.8125,-6.));
#7792=CARTESIAN_POINT('Ctrl Pts',(0.688977411814208,61.8038877823523,-6.));
#7793=CARTESIAN_POINT('Ctrl Pts',(1.37368130809246,61.7953289836488,-5.88131725249645));
#7794=CARTESIAN_POINT('Ctrl Pts',(2.74394904548484,61.7782006369314,-5.39035779280095));
#7795=CARTESIAN_POINT('Ctrl Pts',(3.40815710417449,61.7702927728126,-4.9969670152711));
#7796=CARTESIAN_POINT('Ctrl Pts',(4.56154971839444,61.7520135386179,-3.97431522630718));
#7797=CARTESIAN_POINT('Ctrl Pts',(5.03705640032906,61.7422968962984,-3.35126416771986));
#7798=CARTESIAN_POINT('Ctrl Pts',(5.73213746210445,61.7227031838196,-1.94257977799593));
#7799=CARTESIAN_POINT('Ctrl Pts',(5.93869556354502,61.7130211226562,-1.16744565442734));
#7800=CARTESIAN_POINT('Ctrl Pts',(6.03565876475735,61.6956362955159,0.382514155933625));
#7801=CARTESIAN_POINT('Ctrl Pts',(5.93900543025488,61.6872583429851,1.14180862592295));
#7802=CARTESIAN_POINT('Ctrl Pts',(5.45958655778069,61.6683730231512,2.60956712921656));
#7803=CARTESIAN_POINT('Ctrl Pts',(5.07146103767517,61.6584612628592,3.30109195134678));
#7804=CARTESIAN_POINT('Ctrl Pts',(4.04474262900941,61.6390394316112,4.50242772158962));
#7805=CARTESIAN_POINT('Ctrl Pts',(3.41337234460338,61.6301671543074,4.99806610932519));
#7806=CARTESIAN_POINT('Ctrl Pts',(2.02057663579492,61.6127572079474,5.70114266691254));
#7807=CARTESIAN_POINT('Ctrl Pts',(1.27762644404909,61.6034703305505,5.91214099373319));
#7808=CARTESIAN_POINT('Ctrl Pts',(-0.277349429259922,61.5840331321342,6.04613437437175));
#7809=CARTESIAN_POINT('Ctrl Pts',(-1.0755424524712,61.5740557193441,5.95616320624175));
#7810=CARTESIAN_POINT('Ctrl Pts',(-2.56546866044858,61.5554316417444,5.47815875028546));
#7811=CARTESIAN_POINT('Ctrl Pts',(-3.24601346560067,61.5474695363786,5.10443414682062));
#7812=CARTESIAN_POINT('Ctrl Pts',(-4.43245037929907,61.5293687549667,4.11734525500654));
#7813=CARTESIAN_POINT('Ctrl Pts',(-4.92610044599073,61.5197281188353,3.51179043539488));
#7814=CARTESIAN_POINT('Ctrl Pts',(-5.66570009904181,61.5001323120866,2.12861540595986));
#7815=CARTESIAN_POINT('Ctrl Pts',(-5.89746535371471,61.4903691614763,1.36054391686906));
#7816=CARTESIAN_POINT('Ctrl Pts',(-6.04495653006948,61.4727067352036,-0.1858870628551));
#7817=CARTESIAN_POINT('Ctrl Pts',(-5.97300603582938,61.4645656973602,-0.948294617575622));
#7818=CARTESIAN_POINT('Ctrl Pts',(-5.54204960566922,61.4458464078274,-2.42869570274489));
#7819=CARTESIAN_POINT('Ctrl Pts',(-5.17822300239504,61.435977225973,-3.13031628345293));
#7820=CARTESIAN_POINT('Ctrl Pts',(-4.19451332156246,61.4164832901239,-4.36314389203058));
#7821=CARTESIAN_POINT('Ctrl Pts',(-3.58068615913608,61.4072585769892,-4.87950974091398));
#7822=CARTESIAN_POINT('Ctrl Pts',(-2.21528057083094,61.3901910071353,-5.62800009733629));
#7823=CARTESIAN_POINT('Ctrl Pts',(-1.48257393769345,61.3810321742211,-5.86377086286194));
#7824=CARTESIAN_POINT('Ctrl Pts',(-0.484205589379722,61.3685525698672,-5.98536355884337));
#7825=CARTESIAN_POINT('Ctrl Pts',(-0.241965785432547,61.3655245723179,-5.99999999999999));
#7826=CARTESIAN_POINT('Ctrl Pts',(-5.16947595841089E-14,61.3625,-6.));
#7827=CARTESIAN_POINT('Ctrl Pts',(-6.10622663543836E-15,61.306249998771,
-6.));
#7828=CARTESIAN_POINT('Ctrl Pts',(-0.106729287314065,61.3075841148624,-6.));
#7829=CARTESIAN_POINT('Ctrl Pts',(-0.213561336024365,61.3089195154713,-5.99715225278892));
#7830=CARTESIAN_POINT('Ctrl Pts',(-1.08699672790714,61.3198374578698,-5.95044658308879));
#7831=CARTESIAN_POINT('Ctrl Pts',(-1.83867125547181,61.3292333894644,-5.76269728108951));
#7832=CARTESIAN_POINT('Ctrl Pts',(-3.24720750700701,61.3468400926086,-5.10625765691735));
#7833=CARTESIAN_POINT('Ctrl Pts',(-3.88769465486627,61.3553484105835,-4.63724778150705));
#7834=CARTESIAN_POINT('Ctrl Pts',(-4.95259234219971,61.3745585271075,-3.47751219654718));
#7835=CARTESIAN_POINT('Ctrl Pts',(-5.36610042809721,61.3845038743489,-2.79753937612737));
#7836=CARTESIAN_POINT('Ctrl Pts',(-5.89671680417622,61.4035586161729,-1.34368923227328));
#7837=CARTESIAN_POINT('Ctrl Pts',(-6.01928846149221,61.4122718915949,-0.587285709085823));
#7838=CARTESIAN_POINT('Ctrl Pts',(-5.97479179086783,61.4293623406106,0.965772180516679));
#7839=CARTESIAN_POINT('Ctrl Pts',(-5.79462130968838,61.4389491237747,1.74733979918368));
#7840=CARTESIAN_POINT('Ctrl Pts',(-5.14667212347327,61.4585184100986,3.18097939841526));
#7841=CARTESIAN_POINT('Ctrl Pts',(-4.69063201614918,61.4683038868726,3.82162814362452));
#7842=CARTESIAN_POINT('Ctrl Pts',(-3.57176476423818,61.4867632037124,4.88084848198775));
#7843=CARTESIAN_POINT('Ctrl Pts',(-2.92393676174351,61.4947007892492,5.29440987983458));
#7844=CARTESIAN_POINT('Ctrl Pts',(-1.47181638804433,61.5128522939204,5.87156040110856));
#7845=CARTESIAN_POINT('Ctrl Pts',(-0.675785202994409,61.5228026837335,6.01537749055857));
#7846=CARTESIAN_POINT('Ctrl Pts',(0.894878139798812,61.5424359755185,5.98266182998687));
#7847=CARTESIAN_POINT('Ctrl Pts',(1.65457406399191,61.5519321745709,5.8185434487954));
#7848=CARTESIAN_POINT('Ctrl Pts',(3.07843482283189,61.5697304340564,5.20863678491256));
#7849=CARTESIAN_POINT('Ctrl Pts',(3.72787513446006,61.5779615974826,4.76546028819511));
#7850=CARTESIAN_POINT('Ctrl Pts',(4.8295240529824,61.596953576703,3.64709369739952));
#7851=CARTESIAN_POINT('Ctrl Pts',(5.26771952899154,61.6069204809008,2.97938280197875));
#7852=CARTESIAN_POINT('Ctrl Pts',(5.84880821080874,61.6261354247843,1.53987402507703));
#7853=CARTESIAN_POINT('Ctrl Pts',(5.99683789175222,61.6352220280806,0.785954543753677));
#7854=CARTESIAN_POINT('Ctrl Pts',(6.00319560631724,61.6521014459291,-0.76962865820642));
#7855=CARTESIAN_POINT('Ctrl Pts',(5.84873891680039,61.661546013429,-1.55659478942117));
#7856=CARTESIAN_POINT('Ctrl Pts',(5.2471890916287,61.6810709743493,-3.01292846685));
#7857=CARTESIAN_POINT('Ctrl Pts',(4.81057265753534,61.6909131689183,-3.67003084050065));
#7858=CARTESIAN_POINT('Ctrl Pts',(3.72536844370213,61.7095416668843,-4.76431482595817));
#7859=CARTESIAN_POINT('Ctrl Pts',(3.09286458348203,61.7175891914774,-5.19723457773832));
#7860=CARTESIAN_POINT('Ctrl Pts',(1.66805983060747,61.7353992508884,-5.81797373615802));
#7861=CARTESIAN_POINT('Ctrl Pts',(0.883852492299125,61.7452018426172,-5.98748960197925));
#7862=CARTESIAN_POINT('Ctrl Pts',(0.0596203085914308,61.7555047449136,-5.99977791256666));
#7863=CARTESIAN_POINT('Ctrl Pts',(0.0298052166963125,61.7558774335623,-6.));
#7864=CARTESIAN_POINT('Ctrl Pts',(5.89017058476163E-14,61.756249998771,
-6.));
#7865=CARTESIAN_POINT('Origin',(1.33761810195802E-14,73.,0.));
#7866=CARTESIAN_POINT('',(1.22739989003476E-14,75.,-9.));
#7867=CARTESIAN_POINT('Origin',(1.33761810195802E-14,75.,0.));
#7868=CARTESIAN_POINT('',(1.22739989003476E-14,73.,-9.));
#7869=CARTESIAN_POINT('',(1.22739989003476E-14,73.,-9.));
#7870=CARTESIAN_POINT('Origin',(1.33761810195802E-14,73.,0.));
#7871=CARTESIAN_POINT('Origin',(0.,50.,0.));
#7872=CARTESIAN_POINT('',(-7.34788079488412E-16,75.,-6.));
#7873=CARTESIAN_POINT('',(-7.34788079488412E-16,50.,-6.));
#7874=CARTESIAN_POINT('Origin',(0.,75.,0.));
#7875=CARTESIAN_POINT('Origin',(-65.,400.,0.));
#7876=CARTESIAN_POINT('Origin',(1.33761810195802E-14,73.,0.));
#7877=CARTESIAN_POINT('Origin',(1.33761810195802E-14,75.,0.));
#7878=CARTESIAN_POINT('Origin',(0.,50.,0.));
#7879=CARTESIAN_POINT('Origin',(5.878215178125,50.0703124996927,0.));
#7880=CARTESIAN_POINT('',(5.75643035625,50.1406249993855,0.));
#7881=CARTESIAN_POINT('',(5.878215178125,50.0703124996927,0.));
#7882=CARTESIAN_POINT('',(5.75643035625,50.2531249993855,0.));
#7883=CARTESIAN_POINT('',(5.75643035625,50.1968749993855,0.));
#7884=CARTESIAN_POINT('',(5.878215178125,50.3234374990782,0.));
#7885=CARTESIAN_POINT('Origin',(-2.96955379453125,62.0351562498464,5.14341804793707));
#7886=CARTESIAN_POINT('',(-3.,62.,5.19615242270663));
#7887=CARTESIAN_POINT('',(-2.878215178125,62.2531249993855,4.9852149236284));
#7888=CARTESIAN_POINT('Ctrl Pts',(5.75643035625,50.1406249993855,0.));
#7889=CARTESIAN_POINT('Ctrl Pts',(5.75643035625,50.1781249993855,-3.32347661575227));
#7890=CARTESIAN_POINT('Ctrl Pts',(2.878215178125,50.2156249993855,-4.9852149236284));
#7891=CARTESIAN_POINT('Ctrl Pts',(4.0700849995221E-16,50.2531249993855,
-6.64695323150454));
#7892=CARTESIAN_POINT('Ctrl Pts',(-2.878215178125,50.2906249993855,-4.9852149236284));
#7893=CARTESIAN_POINT('Ctrl Pts',(-5.75643035625,50.3281249993855,-3.32347661575227));
#7894=CARTESIAN_POINT('Ctrl Pts',(-5.75643035625,50.3656249993855,-7.04959401029622E-16));
#7895=CARTESIAN_POINT('Ctrl Pts',(-5.75643035625,50.4031249993855,3.32347661575227));
#7896=CARTESIAN_POINT('Ctrl Pts',(-2.878215178125,50.4406249993855,4.9852149236284));
#7897=CARTESIAN_POINT('Ctrl Pts',(-1.22102549985663E-15,50.4781249993855,
6.64695323150454));
#7898=CARTESIAN_POINT('Ctrl Pts',(2.878215178125,50.5156249993855,4.98521492362841));
#7899=CARTESIAN_POINT('Ctrl Pts',(5.75643035625,50.5531249993855,3.32347661575227));
#7900=CARTESIAN_POINT('Ctrl Pts',(5.75643035625,50.5906249993855,0.));
#7901=CARTESIAN_POINT('Ctrl Pts',(5.75643035625,50.6281249993855,-3.32347661575227));
#7902=CARTESIAN_POINT('Ctrl Pts',(2.878215178125,50.6656249993855,-4.9852149236284));
#7903=CARTESIAN_POINT('Ctrl Pts',(4.0700849995221E-16,50.7031249993855,
-6.64695323150454));
#7904=CARTESIAN_POINT('Ctrl Pts',(-2.878215178125,50.7406249993855,-4.9852149236284));
#7905=CARTESIAN_POINT('Ctrl Pts',(-5.75643035625,50.7781249993855,-3.32347661575227));
#7906=CARTESIAN_POINT('Ctrl Pts',(-5.75643035625,50.8156249993855,-7.04959401029622E-16));
#7907=CARTESIAN_POINT('Ctrl Pts',(-5.75643035625,50.8531249993855,3.32347661575227));
#7908=CARTESIAN_POINT('Ctrl Pts',(-2.878215178125,50.8906249993855,4.9852149236284));
#7909=CARTESIAN_POINT('Ctrl Pts',(-1.22102549985663E-15,50.9281249993855,
6.64695323150454));
#7910=CARTESIAN_POINT('Ctrl Pts',(2.878215178125,50.9656249993855,4.98521492362841));
#7911=CARTESIAN_POINT('Ctrl Pts',(5.75643035625,51.0031249993855,3.32347661575227));
#7912=CARTESIAN_POINT('Ctrl Pts',(5.75643035625,51.0406249993855,0.));
#7913=CARTESIAN_POINT('Ctrl Pts',(5.75643035625,51.0781249993855,-3.32347661575227));
#7914=CARTESIAN_POINT('Ctrl Pts',(2.878215178125,51.1156249993855,-4.9852149236284));
#7915=CARTESIAN_POINT('Ctrl Pts',(4.0700849995221E-16,51.1531249993855,
-6.64695323150454));
#7916=CARTESIAN_POINT('Ctrl Pts',(-2.878215178125,51.1906249993855,-4.9852149236284));
#7917=CARTESIAN_POINT('Ctrl Pts',(-5.75643035625,51.2281249993855,-3.32347661575227));
#7918=CARTESIAN_POINT('Ctrl Pts',(-5.75643035625,51.2656249993855,-7.04959401029622E-16));
#7919=CARTESIAN_POINT('Ctrl Pts',(-5.75643035625,51.3031249993855,3.32347661575227));
#7920=CARTESIAN_POINT('Ctrl Pts',(-2.878215178125,51.3406249993855,4.9852149236284));
#7921=CARTESIAN_POINT('Ctrl Pts',(-1.22102549985663E-15,51.3781249993855,
6.64695323150454));
#7922=CARTESIAN_POINT('Ctrl Pts',(2.878215178125,51.4156249993855,4.98521492362841));
#7923=CARTESIAN_POINT('Ctrl Pts',(5.75643035625,51.4531249993855,3.32347661575227));
#7924=CARTESIAN_POINT('Ctrl Pts',(5.75643035625,51.4906249993855,0.));
#7925=CARTESIAN_POINT('Ctrl Pts',(5.75643035625,51.5281249993855,-3.32347661575227));
#7926=CARTESIAN_POINT('Ctrl Pts',(2.878215178125,51.5656249993855,-4.9852149236284));
#7927=CARTESIAN_POINT('Ctrl Pts',(4.0700849995221E-16,51.6031249993855,
-6.64695323150454));
#7928=CARTESIAN_POINT('Ctrl Pts',(-2.878215178125,51.6406249993855,-4.9852149236284));
#7929=CARTESIAN_POINT('Ctrl Pts',(-5.75643035625,51.6781249993855,-3.32347661575227));
#7930=CARTESIAN_POINT('Ctrl Pts',(-5.75643035625,51.7156249993855,-7.04959401029622E-16));
#7931=CARTESIAN_POINT('Ctrl Pts',(-5.75643035625,51.7531249993855,3.32347661575227));
#7932=CARTESIAN_POINT('Ctrl Pts',(-2.878215178125,51.7906249993855,4.9852149236284));
#7933=CARTESIAN_POINT('Ctrl Pts',(-1.22102549985663E-15,51.8281249993855,
6.64695323150454));
#7934=CARTESIAN_POINT('Ctrl Pts',(2.878215178125,51.8656249993855,4.98521492362841));
#7935=CARTESIAN_POINT('Ctrl Pts',(5.75643035625,51.9031249993855,3.32347661575227));
#7936=CARTESIAN_POINT('Ctrl Pts',(5.75643035625,51.9406249993855,0.));
#7937=CARTESIAN_POINT('Ctrl Pts',(5.75643035625,51.9781249993855,-3.32347661575227));
#7938=CARTESIAN_POINT('Ctrl Pts',(2.878215178125,52.0156249993855,-4.9852149236284));
#7939=CARTESIAN_POINT('Ctrl Pts',(4.0700849995221E-16,52.0531249993855,
-6.64695323150454));
#7940=CARTESIAN_POINT('Ctrl Pts',(-2.878215178125,52.0906249993855,-4.9852149236284));
#7941=CARTESIAN_POINT('Ctrl Pts',(-5.75643035625,52.1281249993855,-3.32347661575227));
#7942=CARTESIAN_POINT('Ctrl Pts',(-5.75643035625,52.1656249993855,-7.04959401029622E-16));
#7943=CARTESIAN_POINT('Ctrl Pts',(-5.75643035625,52.2031249993855,3.32347661575227));
#7944=CARTESIAN_POINT('Ctrl Pts',(-2.878215178125,52.2406249993855,4.9852149236284));
#7945=CARTESIAN_POINT('Ctrl Pts',(-1.22102549985663E-15,52.2781249993855,
6.64695323150454));
#7946=CARTESIAN_POINT('Ctrl Pts',(2.878215178125,52.3156249993855,4.98521492362841));
#7947=CARTESIAN_POINT('Ctrl Pts',(5.75643035625,52.3531249993855,3.32347661575227));
#7948=CARTESIAN_POINT('Ctrl Pts',(5.75643035625,52.3906249993855,0.));
#7949=CARTESIAN_POINT('Ctrl Pts',(5.75643035625,52.4281249993855,-3.32347661575227));
#7950=CARTESIAN_POINT('Ctrl Pts',(2.878215178125,52.4656249993855,-4.9852149236284));
#7951=CARTESIAN_POINT('Ctrl Pts',(4.0700849995221E-16,52.5031249993855,
-6.64695323150454));
#7952=CARTESIAN_POINT('Ctrl Pts',(-2.878215178125,52.5406249993855,-4.9852149236284));
#7953=CARTESIAN_POINT('Ctrl Pts',(-5.75643035625,52.5781249993855,-3.32347661575227));
#7954=CARTESIAN_POINT('Ctrl Pts',(-5.75643035625,52.6156249993855,-7.04959401029622E-16));
#7955=CARTESIAN_POINT('Ctrl Pts',(-5.75643035625,52.6531249993855,3.32347661575227));
#7956=CARTESIAN_POINT('Ctrl Pts',(-2.878215178125,52.6906249993855,4.9852149236284));
#7957=CARTESIAN_POINT('Ctrl Pts',(-1.22102549985663E-15,52.7281249993855,
6.64695323150454));
#7958=CARTESIAN_POINT('Ctrl Pts',(2.878215178125,52.7656249993855,4.98521492362841));
#7959=CARTESIAN_POINT('Ctrl Pts',(5.75643035625,52.8031249993855,3.32347661575227));
#7960=CARTESIAN_POINT('Ctrl Pts',(5.75643035625,52.8406249993855,0.));
#7961=CARTESIAN_POINT('Ctrl Pts',(5.75643035625,52.8781249993855,-3.32347661575227));
#7962=CARTESIAN_POINT('Ctrl Pts',(2.878215178125,52.9156249993855,-4.9852149236284));
#7963=CARTESIAN_POINT('Ctrl Pts',(4.0700849995221E-16,52.9531249993855,
-6.64695323150454));
#7964=CARTESIAN_POINT('Ctrl Pts',(-2.878215178125,52.9906249993855,-4.9852149236284));
#7965=CARTESIAN_POINT('Ctrl Pts',(-5.75643035625,53.0281249993855,-3.32347661575227));
#7966=CARTESIAN_POINT('Ctrl Pts',(-5.75643035625,53.0656249993855,-7.04959401029622E-16));
#7967=CARTESIAN_POINT('Ctrl Pts',(-5.75643035625,53.1031249993855,3.32347661575227));
#7968=CARTESIAN_POINT('Ctrl Pts',(-2.878215178125,53.1406249993855,4.9852149236284));
#7969=CARTESIAN_POINT('Ctrl Pts',(-1.22102549985663E-15,53.1781249993855,
6.64695323150454));
#7970=CARTESIAN_POINT('Ctrl Pts',(2.878215178125,53.2156249993855,4.98521492362841));
#7971=CARTESIAN_POINT('Ctrl Pts',(5.75643035625,53.2531249993855,3.32347661575227));
#7972=CARTESIAN_POINT('Ctrl Pts',(5.75643035625,53.2906249993855,0.));
#7973=CARTESIAN_POINT('Ctrl Pts',(5.75643035625,53.3281249993855,-3.32347661575227));
#7974=CARTESIAN_POINT('Ctrl Pts',(2.878215178125,53.3656249993855,-4.9852149236284));
#7975=CARTESIAN_POINT('Ctrl Pts',(4.0700849995221E-16,53.4031249993855,
-6.64695323150454));
#7976=CARTESIAN_POINT('Ctrl Pts',(-2.878215178125,53.4406249993855,-4.9852149236284));
#7977=CARTESIAN_POINT('Ctrl Pts',(-5.75643035625,53.4781249993855,-3.32347661575227));
#7978=CARTESIAN_POINT('Ctrl Pts',(-5.75643035625,53.5156249993855,-7.04959401029622E-16));
#7979=CARTESIAN_POINT('Ctrl Pts',(-5.75643035625,53.5531249993855,3.32347661575227));
#7980=CARTESIAN_POINT('Ctrl Pts',(-2.878215178125,53.5906249993855,4.9852149236284));
#7981=CARTESIAN_POINT('Ctrl Pts',(-1.22102549985663E-15,53.6281249993855,
6.64695323150454));
#7982=CARTESIAN_POINT('Ctrl Pts',(2.878215178125,53.6656249993855,4.98521492362841));
#7983=CARTESIAN_POINT('Ctrl Pts',(5.75643035625,53.7031249993855,3.32347661575227));
#7984=CARTESIAN_POINT('Ctrl Pts',(5.75643035625,53.7406249993855,0.));
#7985=CARTESIAN_POINT('Ctrl Pts',(5.75643035625,53.7781249993855,-3.32347661575227));
#7986=CARTESIAN_POINT('Ctrl Pts',(2.878215178125,53.8156249993855,-4.9852149236284));
#7987=CARTESIAN_POINT('Ctrl Pts',(4.0700849995221E-16,53.8531249993855,
-6.64695323150454));
#7988=CARTESIAN_POINT('Ctrl Pts',(-2.878215178125,53.8906249993855,-4.9852149236284));
#7989=CARTESIAN_POINT('Ctrl Pts',(-5.75643035625,53.9281249993855,-3.32347661575227));
#7990=CARTESIAN_POINT('Ctrl Pts',(-5.75643035625,53.9656249993855,-7.04959401029622E-16));
#7991=CARTESIAN_POINT('Ctrl Pts',(-5.75643035625,54.0031249993855,3.32347661575227));
#7992=CARTESIAN_POINT('Ctrl Pts',(-2.878215178125,54.0406249993855,4.9852149236284));
#7993=CARTESIAN_POINT('Ctrl Pts',(-1.22102549985663E-15,54.0781249993855,
6.64695323150454));
#7994=CARTESIAN_POINT('Ctrl Pts',(2.878215178125,54.1156249993855,4.98521492362841));
#7995=CARTESIAN_POINT('Ctrl Pts',(5.75643035625,54.1531249993855,3.32347661575227));
#7996=CARTESIAN_POINT('Ctrl Pts',(5.75643035625,54.1906249993855,0.));
#7997=CARTESIAN_POINT('Ctrl Pts',(5.75643035625,54.2281249993855,-3.32347661575227));
#7998=CARTESIAN_POINT('Ctrl Pts',(2.878215178125,54.2656249993855,-4.9852149236284));
#7999=CARTESIAN_POINT('Ctrl Pts',(4.0700849995221E-16,54.3031249993855,
-6.64695323150454));
#8000=CARTESIAN_POINT('Ctrl Pts',(-2.878215178125,54.3406249993855,-4.9852149236284));
#8001=CARTESIAN_POINT('Ctrl Pts',(-5.75643035625,54.3781249993855,-3.32347661575227));
#8002=CARTESIAN_POINT('Ctrl Pts',(-5.75643035625,54.4156249993855,-7.04959401029622E-16));
#8003=CARTESIAN_POINT('Ctrl Pts',(-5.75643035625,54.4531249993855,3.32347661575227));
#8004=CARTESIAN_POINT('Ctrl Pts',(-2.878215178125,54.4906249993855,4.9852149236284));
#8005=CARTESIAN_POINT('Ctrl Pts',(-1.22102549985663E-15,54.5281249993855,
6.64695323150454));
#8006=CARTESIAN_POINT('Ctrl Pts',(2.878215178125,54.5656249993855,4.98521492362841));
#8007=CARTESIAN_POINT('Ctrl Pts',(5.75643035625,54.6031249993855,3.32347661575227));
#8008=CARTESIAN_POINT('Ctrl Pts',(5.75643035625,54.6406249993855,0.));
#8009=CARTESIAN_POINT('Ctrl Pts',(5.75643035625,54.6781249993855,-3.32347661575227));
#8010=CARTESIAN_POINT('Ctrl Pts',(2.878215178125,54.7156249993855,-4.9852149236284));
#8011=CARTESIAN_POINT('Ctrl Pts',(4.0700849995221E-16,54.7531249993855,
-6.64695323150454));
#8012=CARTESIAN_POINT('Ctrl Pts',(-2.878215178125,54.7906249993855,-4.9852149236284));
#8013=CARTESIAN_POINT('Ctrl Pts',(-5.75643035625,54.8281249993855,-3.32347661575227));
#8014=CARTESIAN_POINT('Ctrl Pts',(-5.75643035625,54.8656249993855,-7.04959401029622E-16));
#8015=CARTESIAN_POINT('Ctrl Pts',(-5.75643035625,54.9031249993855,3.32347661575227));
#8016=CARTESIAN_POINT('Ctrl Pts',(-2.878215178125,54.9406249993855,4.9852149236284));
#8017=CARTESIAN_POINT('Ctrl Pts',(-1.22102549985663E-15,54.9781249993855,
6.64695323150454));
#8018=CARTESIAN_POINT('Ctrl Pts',(2.878215178125,55.0156249993855,4.98521492362841));
#8019=CARTESIAN_POINT('Ctrl Pts',(5.75643035625,55.0531249993855,3.32347661575227));
#8020=CARTESIAN_POINT('Ctrl Pts',(5.75643035625,55.0906249993855,0.));
#8021=CARTESIAN_POINT('Ctrl Pts',(5.75643035625,55.1281249993855,-3.32347661575227));
#8022=CARTESIAN_POINT('Ctrl Pts',(2.878215178125,55.1656249993855,-4.9852149236284));
#8023=CARTESIAN_POINT('Ctrl Pts',(4.0700849995221E-16,55.2031249993855,
-6.64695323150454));
#8024=CARTESIAN_POINT('Ctrl Pts',(-2.878215178125,55.2406249993855,-4.9852149236284));
#8025=CARTESIAN_POINT('Ctrl Pts',(-5.75643035625,55.2781249993855,-3.32347661575227));
#8026=CARTESIAN_POINT('Ctrl Pts',(-5.75643035625,55.3156249993855,-7.04959401029622E-16));
#8027=CARTESIAN_POINT('Ctrl Pts',(-5.75643035625,55.3531249993855,3.32347661575227));
#8028=CARTESIAN_POINT('Ctrl Pts',(-2.878215178125,55.3906249993855,4.9852149236284));
#8029=CARTESIAN_POINT('Ctrl Pts',(-1.22102549985663E-15,55.4281249993855,
6.64695323150454));
#8030=CARTESIAN_POINT('Ctrl Pts',(2.878215178125,55.4656249993855,4.98521492362841));
#8031=CARTESIAN_POINT('Ctrl Pts',(5.75643035625,55.5031249993855,3.32347661575227));
#8032=CARTESIAN_POINT('Ctrl Pts',(5.75643035625,55.5406249993855,0.));
#8033=CARTESIAN_POINT('Ctrl Pts',(5.75643035625,55.5781249993855,-3.32347661575227));
#8034=CARTESIAN_POINT('Ctrl Pts',(2.878215178125,55.6156249993855,-4.9852149236284));
#8035=CARTESIAN_POINT('Ctrl Pts',(4.0700849995221E-16,55.6531249993855,
-6.64695323150454));
#8036=CARTESIAN_POINT('Ctrl Pts',(-2.878215178125,55.6906249993855,-4.9852149236284));
#8037=CARTESIAN_POINT('Ctrl Pts',(-5.75643035625,55.7281249993855,-3.32347661575227));
#8038=CARTESIAN_POINT('Ctrl Pts',(-5.75643035625,55.7656249993855,-7.04959401029622E-16));
#8039=CARTESIAN_POINT('Ctrl Pts',(-5.75643035625,55.8031249993855,3.32347661575227));
#8040=CARTESIAN_POINT('Ctrl Pts',(-2.878215178125,55.8406249993855,4.9852149236284));
#8041=CARTESIAN_POINT('Ctrl Pts',(-1.22102549985663E-15,55.8781249993855,
6.64695323150454));
#8042=CARTESIAN_POINT('Ctrl Pts',(2.878215178125,55.9156249993855,4.98521492362841));
#8043=CARTESIAN_POINT('Ctrl Pts',(5.75643035625,55.9531249993855,3.32347661575227));
#8044=CARTESIAN_POINT('Ctrl Pts',(5.75643035625,55.9906249993855,0.));
#8045=CARTESIAN_POINT('Ctrl Pts',(5.75643035625,56.0281249993855,-3.32347661575227));
#8046=CARTESIAN_POINT('Ctrl Pts',(2.878215178125,56.0656249993855,-4.9852149236284));
#8047=CARTESIAN_POINT('Ctrl Pts',(4.0700849995221E-16,56.1031249993855,
-6.64695323150454));
#8048=CARTESIAN_POINT('Ctrl Pts',(-2.878215178125,56.1406249993855,-4.9852149236284));
#8049=CARTESIAN_POINT('Ctrl Pts',(-5.75643035625,56.1781249993855,-3.32347661575227));
#8050=CARTESIAN_POINT('Ctrl Pts',(-5.75643035625,56.2156249993855,-7.04959401029622E-16));
#8051=CARTESIAN_POINT('Ctrl Pts',(-5.75643035625,56.2531249993855,3.32347661575227));
#8052=CARTESIAN_POINT('Ctrl Pts',(-2.878215178125,56.2906249993855,4.9852149236284));
#8053=CARTESIAN_POINT('Ctrl Pts',(-1.22102549985663E-15,56.3281249993855,
6.64695323150454));
#8054=CARTESIAN_POINT('Ctrl Pts',(2.878215178125,56.3656249993855,4.98521492362841));
#8055=CARTESIAN_POINT('Ctrl Pts',(5.75643035625,56.4031249993855,3.32347661575227));
#8056=CARTESIAN_POINT('Ctrl Pts',(5.75643035625,56.4406249993855,0.));
#8057=CARTESIAN_POINT('Ctrl Pts',(5.75643035625,56.4781249993855,-3.32347661575227));
#8058=CARTESIAN_POINT('Ctrl Pts',(2.878215178125,56.5156249993855,-4.9852149236284));
#8059=CARTESIAN_POINT('Ctrl Pts',(4.0700849995221E-16,56.5531249993855,
-6.64695323150454));
#8060=CARTESIAN_POINT('Ctrl Pts',(-2.878215178125,56.5906249993855,-4.9852149236284));
#8061=CARTESIAN_POINT('Ctrl Pts',(-5.75643035625,56.6281249993855,-3.32347661575227));
#8062=CARTESIAN_POINT('Ctrl Pts',(-5.75643035625,56.6656249993855,-7.04959401029622E-16));
#8063=CARTESIAN_POINT('Ctrl Pts',(-5.75643035625,56.7031249993855,3.32347661575227));
#8064=CARTESIAN_POINT('Ctrl Pts',(-2.878215178125,56.7406249993855,4.9852149236284));
#8065=CARTESIAN_POINT('Ctrl Pts',(-1.22102549985663E-15,56.7781249993855,
6.64695323150454));
#8066=CARTESIAN_POINT('Ctrl Pts',(2.878215178125,56.8156249993855,4.98521492362841));
#8067=CARTESIAN_POINT('Ctrl Pts',(5.75643035625,56.8531249993855,3.32347661575227));
#8068=CARTESIAN_POINT('Ctrl Pts',(5.75643035625,56.8906249993855,0.));
#8069=CARTESIAN_POINT('Ctrl Pts',(5.75643035625,56.9281249993855,-3.32347661575227));
#8070=CARTESIAN_POINT('Ctrl Pts',(2.878215178125,56.9656249993855,-4.9852149236284));
#8071=CARTESIAN_POINT('Ctrl Pts',(4.0700849995221E-16,57.0031249993855,
-6.64695323150454));
#8072=CARTESIAN_POINT('Ctrl Pts',(-2.878215178125,57.0406249993855,-4.9852149236284));
#8073=CARTESIAN_POINT('Ctrl Pts',(-5.75643035625,57.0781249993855,-3.32347661575227));
#8074=CARTESIAN_POINT('Ctrl Pts',(-5.75643035625,57.1156249993855,-7.04959401029622E-16));
#8075=CARTESIAN_POINT('Ctrl Pts',(-5.75643035625,57.1531249993855,3.32347661575227));
#8076=CARTESIAN_POINT('Ctrl Pts',(-2.878215178125,57.1906249993855,4.9852149236284));
#8077=CARTESIAN_POINT('Ctrl Pts',(-1.22102549985663E-15,57.2281249993855,
6.64695323150454));
#8078=CARTESIAN_POINT('Ctrl Pts',(2.878215178125,57.2656249993855,4.98521492362841));
#8079=CARTESIAN_POINT('Ctrl Pts',(5.75643035625,57.3031249993855,3.32347661575227));
#8080=CARTESIAN_POINT('Ctrl Pts',(5.75643035625,57.3406249993855,0.));
#8081=CARTESIAN_POINT('Ctrl Pts',(5.75643035625,57.3781249993855,-3.32347661575227));
#8082=CARTESIAN_POINT('Ctrl Pts',(2.878215178125,57.4156249993855,-4.9852149236284));
#8083=CARTESIAN_POINT('Ctrl Pts',(4.0700849995221E-16,57.4531249993855,
-6.64695323150454));
#8084=CARTESIAN_POINT('Ctrl Pts',(-2.878215178125,57.4906249993855,-4.9852149236284));
#8085=CARTESIAN_POINT('Ctrl Pts',(-5.75643035625,57.5281249993855,-3.32347661575227));
#8086=CARTESIAN_POINT('Ctrl Pts',(-5.75643035625,57.5656249993855,-7.04959401029622E-16));
#8087=CARTESIAN_POINT('Ctrl Pts',(-5.75643035625,57.6031249993855,3.32347661575227));
#8088=CARTESIAN_POINT('Ctrl Pts',(-2.878215178125,57.6406249993855,4.9852149236284));
#8089=CARTESIAN_POINT('Ctrl Pts',(-1.22102549985663E-15,57.6781249993855,
6.64695323150454));
#8090=CARTESIAN_POINT('Ctrl Pts',(2.878215178125,57.7156249993855,4.98521492362841));
#8091=CARTESIAN_POINT('Ctrl Pts',(5.75643035625,57.7531249993855,3.32347661575227));
#8092=CARTESIAN_POINT('Ctrl Pts',(5.75643035625,57.7906249993855,0.));
#8093=CARTESIAN_POINT('Ctrl Pts',(5.75643035625,57.8281249993855,-3.32347661575227));
#8094=CARTESIAN_POINT('Ctrl Pts',(2.878215178125,57.8656249993855,-4.9852149236284));
#8095=CARTESIAN_POINT('Ctrl Pts',(4.0700849995221E-16,57.9031249993855,
-6.64695323150454));
#8096=CARTESIAN_POINT('Ctrl Pts',(-2.878215178125,57.9406249993855,-4.9852149236284));
#8097=CARTESIAN_POINT('Ctrl Pts',(-5.75643035625,57.9781249993855,-3.32347661575227));
#8098=CARTESIAN_POINT('Ctrl Pts',(-5.75643035625,58.0156249993855,-7.04959401029622E-16));
#8099=CARTESIAN_POINT('Ctrl Pts',(-5.75643035625,58.0531249993855,3.32347661575227));
#8100=CARTESIAN_POINT('Ctrl Pts',(-2.878215178125,58.0906249993855,4.9852149236284));
#8101=CARTESIAN_POINT('Ctrl Pts',(-1.22102549985663E-15,58.1281249993855,
6.64695323150454));
#8102=CARTESIAN_POINT('Ctrl Pts',(2.878215178125,58.1656249993855,4.98521492362841));
#8103=CARTESIAN_POINT('Ctrl Pts',(5.75643035625,58.2031249993855,3.32347661575227));
#8104=CARTESIAN_POINT('Ctrl Pts',(5.75643035625,58.2406249993855,0.));
#8105=CARTESIAN_POINT('Ctrl Pts',(5.75643035625,58.2781249993855,-3.32347661575227));
#8106=CARTESIAN_POINT('Ctrl Pts',(2.878215178125,58.3156249993855,-4.9852149236284));
#8107=CARTESIAN_POINT('Ctrl Pts',(4.0700849995221E-16,58.3531249993855,
-6.64695323150454));
#8108=CARTESIAN_POINT('Ctrl Pts',(-2.878215178125,58.3906249993855,-4.9852149236284));
#8109=CARTESIAN_POINT('Ctrl Pts',(-5.75643035625,58.4281249993855,-3.32347661575227));
#8110=CARTESIAN_POINT('Ctrl Pts',(-5.75643035625,58.4656249993855,-7.04959401029622E-16));
#8111=CARTESIAN_POINT('Ctrl Pts',(-5.75643035625,58.5031249993855,3.32347661575227));
#8112=CARTESIAN_POINT('Ctrl Pts',(-2.878215178125,58.5406249993855,4.9852149236284));
#8113=CARTESIAN_POINT('Ctrl Pts',(-1.22102549985663E-15,58.5781249993855,
6.64695323150454));
#8114=CARTESIAN_POINT('Ctrl Pts',(2.878215178125,58.6156249993855,4.98521492362841));
#8115=CARTESIAN_POINT('Ctrl Pts',(5.75643035625,58.6531249993855,3.32347661575227));
#8116=CARTESIAN_POINT('Ctrl Pts',(5.75643035625,58.6906249993855,0.));
#8117=CARTESIAN_POINT('Ctrl Pts',(5.75643035625,58.7281249993855,-3.32347661575227));
#8118=CARTESIAN_POINT('Ctrl Pts',(2.878215178125,58.7656249993855,-4.9852149236284));
#8119=CARTESIAN_POINT('Ctrl Pts',(4.0700849995221E-16,58.8031249993855,
-6.64695323150454));
#8120=CARTESIAN_POINT('Ctrl Pts',(-2.878215178125,58.8406249993855,-4.9852149236284));
#8121=CARTESIAN_POINT('Ctrl Pts',(-5.75643035625,58.8781249993855,-3.32347661575227));
#8122=CARTESIAN_POINT('Ctrl Pts',(-5.75643035625,58.9156249993855,-7.04959401029622E-16));
#8123=CARTESIAN_POINT('Ctrl Pts',(-5.75643035625,58.9531249993855,3.32347661575227));
#8124=CARTESIAN_POINT('Ctrl Pts',(-2.878215178125,58.9906249993855,4.9852149236284));
#8125=CARTESIAN_POINT('Ctrl Pts',(-1.22102549985663E-15,59.0281249993855,
6.64695323150454));
#8126=CARTESIAN_POINT('Ctrl Pts',(2.878215178125,59.0656249993855,4.98521492362841));
#8127=CARTESIAN_POINT('Ctrl Pts',(5.75643035625,59.1031249993855,3.32347661575227));
#8128=CARTESIAN_POINT('Ctrl Pts',(5.75643035625,59.1406249993855,0.));
#8129=CARTESIAN_POINT('Ctrl Pts',(5.75643035625,59.1781249993855,-3.32347661575227));
#8130=CARTESIAN_POINT('Ctrl Pts',(2.878215178125,59.2156249993855,-4.9852149236284));
#8131=CARTESIAN_POINT('Ctrl Pts',(4.0700849995221E-16,59.2531249993855,
-6.64695323150454));
#8132=CARTESIAN_POINT('Ctrl Pts',(-2.878215178125,59.2906249993855,-4.9852149236284));
#8133=CARTESIAN_POINT('Ctrl Pts',(-5.75643035625,59.3281249993855,-3.32347661575227));
#8134=CARTESIAN_POINT('Ctrl Pts',(-5.75643035625,59.3656249993855,-7.04959401029622E-16));
#8135=CARTESIAN_POINT('Ctrl Pts',(-5.75643035625,59.4031249993855,3.32347661575227));
#8136=CARTESIAN_POINT('Ctrl Pts',(-2.878215178125,59.4406249993855,4.9852149236284));
#8137=CARTESIAN_POINT('Ctrl Pts',(-1.22102549985663E-15,59.4781249993855,
6.64695323150454));
#8138=CARTESIAN_POINT('Ctrl Pts',(2.878215178125,59.5156249993855,4.98521492362841));
#8139=CARTESIAN_POINT('Ctrl Pts',(5.75643035625,59.5531249993855,3.32347661575227));
#8140=CARTESIAN_POINT('Ctrl Pts',(5.75643035625,59.5906249993855,0.));
#8141=CARTESIAN_POINT('Ctrl Pts',(5.75643035625,59.6281249993855,-3.32347661575227));
#8142=CARTESIAN_POINT('Ctrl Pts',(2.878215178125,59.6656249993855,-4.9852149236284));
#8143=CARTESIAN_POINT('Ctrl Pts',(4.0700849995221E-16,59.7031249993855,
-6.64695323150454));
#8144=CARTESIAN_POINT('Ctrl Pts',(-2.878215178125,59.7406249993855,-4.9852149236284));
#8145=CARTESIAN_POINT('Ctrl Pts',(-5.75643035625,59.7781249993855,-3.32347661575227));
#8146=CARTESIAN_POINT('Ctrl Pts',(-5.75643035625,59.8156249993855,-7.04959401029622E-16));
#8147=CARTESIAN_POINT('Ctrl Pts',(-5.75643035625,59.8531249993855,3.32347661575227));
#8148=CARTESIAN_POINT('Ctrl Pts',(-2.878215178125,59.8906249993855,4.9852149236284));
#8149=CARTESIAN_POINT('Ctrl Pts',(-1.22102549985663E-15,59.9281249993855,
6.64695323150454));
#8150=CARTESIAN_POINT('Ctrl Pts',(2.878215178125,59.9656249993855,4.98521492362841));
#8151=CARTESIAN_POINT('Ctrl Pts',(5.75643035625,60.0031249993855,3.32347661575227));
#8152=CARTESIAN_POINT('Ctrl Pts',(5.75643035625,60.0406249993855,0.));
#8153=CARTESIAN_POINT('Ctrl Pts',(5.75643035625,60.0781249993855,-3.32347661575227));
#8154=CARTESIAN_POINT('Ctrl Pts',(2.878215178125,60.1156249993855,-4.9852149236284));
#8155=CARTESIAN_POINT('Ctrl Pts',(4.0700849995221E-16,60.1531249993855,
-6.64695323150454));
#8156=CARTESIAN_POINT('Ctrl Pts',(-2.878215178125,60.1906249993855,-4.9852149236284));
#8157=CARTESIAN_POINT('Ctrl Pts',(-5.75643035625,60.2281249993855,-3.32347661575227));
#8158=CARTESIAN_POINT('Ctrl Pts',(-5.75643035625,60.2656249993855,-7.04959401029622E-16));
#8159=CARTESIAN_POINT('Ctrl Pts',(-5.75643035625,60.3031249993855,3.32347661575227));
#8160=CARTESIAN_POINT('Ctrl Pts',(-2.878215178125,60.3406249993855,4.9852149236284));
#8161=CARTESIAN_POINT('Ctrl Pts',(-1.22102549985663E-15,60.3781249993855,
6.64695323150454));
#8162=CARTESIAN_POINT('Ctrl Pts',(2.878215178125,60.4156249993855,4.98521492362841));
#8163=CARTESIAN_POINT('Ctrl Pts',(5.75643035625,60.4531249993855,3.32347661575227));
#8164=CARTESIAN_POINT('Ctrl Pts',(5.75643035625,60.4906249993855,0.));
#8165=CARTESIAN_POINT('Ctrl Pts',(5.75643035625,60.5281249993855,-3.32347661575227));
#8166=CARTESIAN_POINT('Ctrl Pts',(2.878215178125,60.5656249993855,-4.9852149236284));
#8167=CARTESIAN_POINT('Ctrl Pts',(4.0700849995221E-16,60.6031249993855,
-6.64695323150454));
#8168=CARTESIAN_POINT('Ctrl Pts',(-2.878215178125,60.6406249993855,-4.9852149236284));
#8169=CARTESIAN_POINT('Ctrl Pts',(-5.75643035625,60.6781249993855,-3.32347661575227));
#8170=CARTESIAN_POINT('Ctrl Pts',(-5.75643035625,60.7156249993855,-7.04959401029622E-16));
#8171=CARTESIAN_POINT('Ctrl Pts',(-5.75643035625,60.7531249993855,3.32347661575227));
#8172=CARTESIAN_POINT('Ctrl Pts',(-2.878215178125,60.7906249993855,4.9852149236284));
#8173=CARTESIAN_POINT('Ctrl Pts',(-1.22102549985663E-15,60.8281249993855,
6.64695323150454));
#8174=CARTESIAN_POINT('Ctrl Pts',(2.878215178125,60.8656249993855,4.98521492362841));
#8175=CARTESIAN_POINT('Ctrl Pts',(5.75643035625,60.9031249993855,3.32347661575227));
#8176=CARTESIAN_POINT('Ctrl Pts',(5.75643035625,60.9406249993855,0.));
#8177=CARTESIAN_POINT('Ctrl Pts',(5.75643035625,60.9781249993855,-3.32347661575227));
#8178=CARTESIAN_POINT('Ctrl Pts',(2.878215178125,61.0156249993855,-4.9852149236284));
#8179=CARTESIAN_POINT('Ctrl Pts',(4.0700849995221E-16,61.0531249993855,
-6.64695323150454));
#8180=CARTESIAN_POINT('Ctrl Pts',(-2.878215178125,61.0906249993855,-4.9852149236284));
#8181=CARTESIAN_POINT('Ctrl Pts',(-5.75643035625,61.1281249993855,-3.32347661575227));
#8182=CARTESIAN_POINT('Ctrl Pts',(-5.75643035625,61.1656249993855,-7.04959401029622E-16));
#8183=CARTESIAN_POINT('Ctrl Pts',(-5.75643035625,61.2031249993855,3.32347661575227));
#8184=CARTESIAN_POINT('Ctrl Pts',(-2.878215178125,61.2406249993855,4.9852149236284));
#8185=CARTESIAN_POINT('Ctrl Pts',(-1.22102549985663E-15,61.2781249993855,
6.64695323150454));
#8186=CARTESIAN_POINT('Ctrl Pts',(2.878215178125,61.3156249993855,4.98521492362841));
#8187=CARTESIAN_POINT('Ctrl Pts',(5.75643035625,61.3531249993855,3.32347661575227));
#8188=CARTESIAN_POINT('Ctrl Pts',(5.75643035625,61.3906249993855,0.));
#8189=CARTESIAN_POINT('Ctrl Pts',(5.75643035625,61.4281249993855,-3.32347661575227));
#8190=CARTESIAN_POINT('Ctrl Pts',(2.878215178125,61.4656249993855,-4.9852149236284));
#8191=CARTESIAN_POINT('Ctrl Pts',(4.0700849995221E-16,61.5031249993855,
-6.64695323150454));
#8192=CARTESIAN_POINT('Ctrl Pts',(-2.878215178125,61.5406249993855,-4.9852149236284));
#8193=CARTESIAN_POINT('Ctrl Pts',(-5.75643035625,61.5781249993855,-3.32347661575227));
#8194=CARTESIAN_POINT('Ctrl Pts',(-5.75643035625,61.6156249993855,-7.04959401029622E-16));
#8195=CARTESIAN_POINT('Ctrl Pts',(-5.75643035625,61.6531249993855,3.32347661575227));
#8196=CARTESIAN_POINT('Ctrl Pts',(-2.878215178125,61.6906249993855,4.9852149236284));
#8197=CARTESIAN_POINT('Ctrl Pts',(-1.22102549985663E-15,61.7281249993855,
6.64695323150454));
#8198=CARTESIAN_POINT('Ctrl Pts',(2.878215178125,61.7656249993855,4.98521492362841));
#8199=CARTESIAN_POINT('Ctrl Pts',(5.75643035625,61.8031249993855,3.32347661575227));
#8200=CARTESIAN_POINT('Ctrl Pts',(5.75643035625,61.8406249993855,0.));
#8201=CARTESIAN_POINT('Ctrl Pts',(5.75643035625,61.8781249993855,-3.32347661575227));
#8202=CARTESIAN_POINT('Ctrl Pts',(2.878215178125,61.9156249993855,-4.9852149236284));
#8203=CARTESIAN_POINT('Ctrl Pts',(4.0700849995221E-16,61.9531249993855,
-6.64695323150454));
#8204=CARTESIAN_POINT('Ctrl Pts',(-2.878215178125,61.9906249993855,-4.9852149236284));
#8205=CARTESIAN_POINT('Ctrl Pts',(-5.75643035625,62.0281249993855,-3.32347661575227));
#8206=CARTESIAN_POINT('Ctrl Pts',(-5.75643035625,62.0656249993855,-7.04959401029622E-16));
#8207=CARTESIAN_POINT('Ctrl Pts',(-5.75643035625,62.1031249993855,3.32347661575227));
#8208=CARTESIAN_POINT('Ctrl Pts',(-2.878215178125,62.1406249993855,4.9852149236284));
#8209=CARTESIAN_POINT('Ctrl Pts',(6.,50.,0.));
#8210=CARTESIAN_POINT('Ctrl Pts',(6.,50.0375,-3.46410161513775));
#8211=CARTESIAN_POINT('Ctrl Pts',(3.,50.075,-5.19615242270663));
#8212=CARTESIAN_POINT('Ctrl Pts',(4.24230095489963E-16,50.1125,-6.92820323027551));
#8213=CARTESIAN_POINT('Ctrl Pts',(-3.,50.15,-5.19615242270663));
#8214=CARTESIAN_POINT('Ctrl Pts',(-6.,50.1875,-3.46410161513776));
#8215=CARTESIAN_POINT('Ctrl Pts',(-6.,50.225,-7.34788079488412E-16));
#8216=CARTESIAN_POINT('Ctrl Pts',(-6.,50.2625,3.46410161513775));
#8217=CARTESIAN_POINT('Ctrl Pts',(-3.,50.3,5.19615242270663));
#8218=CARTESIAN_POINT('Ctrl Pts',(-1.27269028646989E-15,50.3375,6.92820323027551));
#8219=CARTESIAN_POINT('Ctrl Pts',(3.,50.375,5.19615242270663));
#8220=CARTESIAN_POINT('Ctrl Pts',(6.,50.4125,3.46410161513776));
#8221=CARTESIAN_POINT('Ctrl Pts',(6.,50.45,0.));
#8222=CARTESIAN_POINT('Ctrl Pts',(6.,50.4875,-3.46410161513775));
#8223=CARTESIAN_POINT('Ctrl Pts',(3.,50.525,-5.19615242270663));
#8224=CARTESIAN_POINT('Ctrl Pts',(4.24230095489963E-16,50.5625,-6.92820323027551));
#8225=CARTESIAN_POINT('Ctrl Pts',(-3.,50.6,-5.19615242270663));
#8226=CARTESIAN_POINT('Ctrl Pts',(-6.,50.6375,-3.46410161513776));
#8227=CARTESIAN_POINT('Ctrl Pts',(-6.,50.675,-7.34788079488412E-16));
#8228=CARTESIAN_POINT('Ctrl Pts',(-6.,50.7125,3.46410161513775));
#8229=CARTESIAN_POINT('Ctrl Pts',(-3.,50.75,5.19615242270663));
#8230=CARTESIAN_POINT('Ctrl Pts',(-1.27269028646989E-15,50.7875,6.92820323027551));
#8231=CARTESIAN_POINT('Ctrl Pts',(3.,50.825,5.19615242270663));
#8232=CARTESIAN_POINT('Ctrl Pts',(6.,50.8625,3.46410161513776));
#8233=CARTESIAN_POINT('Ctrl Pts',(6.,50.9,0.));
#8234=CARTESIAN_POINT('Ctrl Pts',(6.,50.9375,-3.46410161513775));
#8235=CARTESIAN_POINT('Ctrl Pts',(3.,50.975,-5.19615242270663));
#8236=CARTESIAN_POINT('Ctrl Pts',(4.24230095489963E-16,51.0125,-6.92820323027551));
#8237=CARTESIAN_POINT('Ctrl Pts',(-3.,51.05,-5.19615242270663));
#8238=CARTESIAN_POINT('Ctrl Pts',(-6.,51.0875,-3.46410161513776));
#8239=CARTESIAN_POINT('Ctrl Pts',(-6.,51.125,-7.34788079488412E-16));
#8240=CARTESIAN_POINT('Ctrl Pts',(-6.,51.1625,3.46410161513775));
#8241=CARTESIAN_POINT('Ctrl Pts',(-3.,51.2,5.19615242270663));
#8242=CARTESIAN_POINT('Ctrl Pts',(-1.27269028646989E-15,51.2375,6.92820323027551));
#8243=CARTESIAN_POINT('Ctrl Pts',(3.,51.275,5.19615242270663));
#8244=CARTESIAN_POINT('Ctrl Pts',(6.,51.3125,3.46410161513776));
#8245=CARTESIAN_POINT('Ctrl Pts',(6.,51.35,0.));
#8246=CARTESIAN_POINT('Ctrl Pts',(6.,51.3875,-3.46410161513775));
#8247=CARTESIAN_POINT('Ctrl Pts',(3.,51.425,-5.19615242270663));
#8248=CARTESIAN_POINT('Ctrl Pts',(4.24230095489963E-16,51.4625,-6.92820323027551));
#8249=CARTESIAN_POINT('Ctrl Pts',(-3.,51.5,-5.19615242270663));
#8250=CARTESIAN_POINT('Ctrl Pts',(-6.,51.5375,-3.46410161513776));
#8251=CARTESIAN_POINT('Ctrl Pts',(-6.,51.575,-7.34788079488412E-16));
#8252=CARTESIAN_POINT('Ctrl Pts',(-6.,51.6125,3.46410161513775));
#8253=CARTESIAN_POINT('Ctrl Pts',(-3.,51.65,5.19615242270663));
#8254=CARTESIAN_POINT('Ctrl Pts',(-1.27269028646989E-15,51.6875,6.92820323027551));
#8255=CARTESIAN_POINT('Ctrl Pts',(3.,51.725,5.19615242270663));
#8256=CARTESIAN_POINT('Ctrl Pts',(6.,51.7625,3.46410161513776));
#8257=CARTESIAN_POINT('Ctrl Pts',(6.,51.8,0.));
#8258=CARTESIAN_POINT('Ctrl Pts',(6.,51.8375,-3.46410161513775));
#8259=CARTESIAN_POINT('Ctrl Pts',(3.,51.875,-5.19615242270663));
#8260=CARTESIAN_POINT('Ctrl Pts',(4.24230095489963E-16,51.9125,-6.92820323027551));
#8261=CARTESIAN_POINT('Ctrl Pts',(-3.,51.95,-5.19615242270663));
#8262=CARTESIAN_POINT('Ctrl Pts',(-6.,51.9875,-3.46410161513776));
#8263=CARTESIAN_POINT('Ctrl Pts',(-6.,52.025,-7.34788079488412E-16));
#8264=CARTESIAN_POINT('Ctrl Pts',(-6.,52.0625,3.46410161513775));
#8265=CARTESIAN_POINT('Ctrl Pts',(-3.,52.1,5.19615242270663));
#8266=CARTESIAN_POINT('Ctrl Pts',(-1.27269028646989E-15,52.1375,6.92820323027551));
#8267=CARTESIAN_POINT('Ctrl Pts',(3.,52.175,5.19615242270663));
#8268=CARTESIAN_POINT('Ctrl Pts',(6.,52.2125,3.46410161513776));
#8269=CARTESIAN_POINT('Ctrl Pts',(6.,52.25,0.));
#8270=CARTESIAN_POINT('Ctrl Pts',(6.,52.2875,-3.46410161513775));
#8271=CARTESIAN_POINT('Ctrl Pts',(3.,52.325,-5.19615242270663));
#8272=CARTESIAN_POINT('Ctrl Pts',(4.24230095489963E-16,52.3625,-6.92820323027551));
#8273=CARTESIAN_POINT('Ctrl Pts',(-3.,52.4,-5.19615242270663));
#8274=CARTESIAN_POINT('Ctrl Pts',(-6.,52.4375,-3.46410161513776));
#8275=CARTESIAN_POINT('Ctrl Pts',(-6.,52.475,-7.34788079488412E-16));
#8276=CARTESIAN_POINT('Ctrl Pts',(-6.,52.5125,3.46410161513775));
#8277=CARTESIAN_POINT('Ctrl Pts',(-3.,52.55,5.19615242270663));
#8278=CARTESIAN_POINT('Ctrl Pts',(-1.27269028646989E-15,52.5875,6.92820323027551));
#8279=CARTESIAN_POINT('Ctrl Pts',(3.,52.625,5.19615242270663));
#8280=CARTESIAN_POINT('Ctrl Pts',(6.,52.6625,3.46410161513776));
#8281=CARTESIAN_POINT('Ctrl Pts',(6.,52.7,0.));
#8282=CARTESIAN_POINT('Ctrl Pts',(6.,52.7375,-3.46410161513775));
#8283=CARTESIAN_POINT('Ctrl Pts',(3.,52.775,-5.19615242270663));
#8284=CARTESIAN_POINT('Ctrl Pts',(4.24230095489963E-16,52.8125,-6.92820323027551));
#8285=CARTESIAN_POINT('Ctrl Pts',(-3.,52.85,-5.19615242270663));
#8286=CARTESIAN_POINT('Ctrl Pts',(-6.,52.8875,-3.46410161513776));
#8287=CARTESIAN_POINT('Ctrl Pts',(-6.,52.925,-7.34788079488412E-16));
#8288=CARTESIAN_POINT('Ctrl Pts',(-6.,52.9625,3.46410161513775));
#8289=CARTESIAN_POINT('Ctrl Pts',(-3.,53.,5.19615242270663));
#8290=CARTESIAN_POINT('Ctrl Pts',(-1.27269028646989E-15,53.0375,6.92820323027551));
#8291=CARTESIAN_POINT('Ctrl Pts',(3.,53.075,5.19615242270663));
#8292=CARTESIAN_POINT('Ctrl Pts',(6.,53.1125,3.46410161513776));
#8293=CARTESIAN_POINT('Ctrl Pts',(6.,53.15,0.));
#8294=CARTESIAN_POINT('Ctrl Pts',(6.,53.1875,-3.46410161513775));
#8295=CARTESIAN_POINT('Ctrl Pts',(3.,53.225,-5.19615242270663));
#8296=CARTESIAN_POINT('Ctrl Pts',(4.24230095489963E-16,53.2625,-6.92820323027551));
#8297=CARTESIAN_POINT('Ctrl Pts',(-3.,53.3,-5.19615242270663));
#8298=CARTESIAN_POINT('Ctrl Pts',(-6.,53.3375,-3.46410161513776));
#8299=CARTESIAN_POINT('Ctrl Pts',(-6.,53.375,-7.34788079488412E-16));
#8300=CARTESIAN_POINT('Ctrl Pts',(-6.,53.4125,3.46410161513775));
#8301=CARTESIAN_POINT('Ctrl Pts',(-3.,53.45,5.19615242270663));
#8302=CARTESIAN_POINT('Ctrl Pts',(-1.27269028646989E-15,53.4875,6.92820323027551));
#8303=CARTESIAN_POINT('Ctrl Pts',(3.,53.525,5.19615242270663));
#8304=CARTESIAN_POINT('Ctrl Pts',(6.,53.5625,3.46410161513776));
#8305=CARTESIAN_POINT('Ctrl Pts',(6.,53.6,0.));
#8306=CARTESIAN_POINT('Ctrl Pts',(6.,53.6375,-3.46410161513775));
#8307=CARTESIAN_POINT('Ctrl Pts',(3.,53.675,-5.19615242270663));
#8308=CARTESIAN_POINT('Ctrl Pts',(4.24230095489963E-16,53.7125,-6.92820323027551));
#8309=CARTESIAN_POINT('Ctrl Pts',(-3.,53.75,-5.19615242270663));
#8310=CARTESIAN_POINT('Ctrl Pts',(-6.,53.7875,-3.46410161513776));
#8311=CARTESIAN_POINT('Ctrl Pts',(-6.,53.825,-7.34788079488412E-16));
#8312=CARTESIAN_POINT('Ctrl Pts',(-6.,53.8625,3.46410161513775));
#8313=CARTESIAN_POINT('Ctrl Pts',(-3.,53.9,5.19615242270663));
#8314=CARTESIAN_POINT('Ctrl Pts',(-1.27269028646989E-15,53.9375,6.92820323027551));
#8315=CARTESIAN_POINT('Ctrl Pts',(3.,53.975,5.19615242270663));
#8316=CARTESIAN_POINT('Ctrl Pts',(6.,54.0125,3.46410161513776));
#8317=CARTESIAN_POINT('Ctrl Pts',(6.,54.05,0.));
#8318=CARTESIAN_POINT('Ctrl Pts',(6.,54.0875,-3.46410161513775));
#8319=CARTESIAN_POINT('Ctrl Pts',(3.,54.125,-5.19615242270663));
#8320=CARTESIAN_POINT('Ctrl Pts',(4.24230095489963E-16,54.1625,-6.92820323027551));
#8321=CARTESIAN_POINT('Ctrl Pts',(-3.,54.2,-5.19615242270663));
#8322=CARTESIAN_POINT('Ctrl Pts',(-6.,54.2375,-3.46410161513776));
#8323=CARTESIAN_POINT('Ctrl Pts',(-6.,54.275,-7.34788079488412E-16));
#8324=CARTESIAN_POINT('Ctrl Pts',(-6.,54.3125,3.46410161513775));
#8325=CARTESIAN_POINT('Ctrl Pts',(-3.,54.35,5.19615242270663));
#8326=CARTESIAN_POINT('Ctrl Pts',(-1.27269028646989E-15,54.3875,6.92820323027551));
#8327=CARTESIAN_POINT('Ctrl Pts',(3.,54.425,5.19615242270663));
#8328=CARTESIAN_POINT('Ctrl Pts',(6.,54.4625,3.46410161513776));
#8329=CARTESIAN_POINT('Ctrl Pts',(6.,54.5,0.));
#8330=CARTESIAN_POINT('Ctrl Pts',(6.,54.5375,-3.46410161513775));
#8331=CARTESIAN_POINT('Ctrl Pts',(3.,54.575,-5.19615242270663));
#8332=CARTESIAN_POINT('Ctrl Pts',(4.24230095489963E-16,54.6125,-6.92820323027551));
#8333=CARTESIAN_POINT('Ctrl Pts',(-3.,54.65,-5.19615242270663));
#8334=CARTESIAN_POINT('Ctrl Pts',(-6.,54.6875,-3.46410161513776));
#8335=CARTESIAN_POINT('Ctrl Pts',(-6.,54.725,-7.34788079488412E-16));
#8336=CARTESIAN_POINT('Ctrl Pts',(-6.,54.7625,3.46410161513775));
#8337=CARTESIAN_POINT('Ctrl Pts',(-3.,54.8,5.19615242270663));
#8338=CARTESIAN_POINT('Ctrl Pts',(-1.27269028646989E-15,54.8375,6.92820323027551));
#8339=CARTESIAN_POINT('Ctrl Pts',(3.,54.875,5.19615242270663));
#8340=CARTESIAN_POINT('Ctrl Pts',(6.,54.9125,3.46410161513776));
#8341=CARTESIAN_POINT('Ctrl Pts',(6.,54.95,0.));
#8342=CARTESIAN_POINT('Ctrl Pts',(6.,54.9875,-3.46410161513775));
#8343=CARTESIAN_POINT('Ctrl Pts',(3.,55.025,-5.19615242270663));
#8344=CARTESIAN_POINT('Ctrl Pts',(4.24230095489963E-16,55.0625,-6.92820323027551));
#8345=CARTESIAN_POINT('Ctrl Pts',(-3.,55.1,-5.19615242270663));
#8346=CARTESIAN_POINT('Ctrl Pts',(-6.,55.1375,-3.46410161513776));
#8347=CARTESIAN_POINT('Ctrl Pts',(-6.,55.175,-7.34788079488412E-16));
#8348=CARTESIAN_POINT('Ctrl Pts',(-6.,55.2125,3.46410161513775));
#8349=CARTESIAN_POINT('Ctrl Pts',(-3.,55.25,5.19615242270663));
#8350=CARTESIAN_POINT('Ctrl Pts',(-1.27269028646989E-15,55.2875,6.92820323027551));
#8351=CARTESIAN_POINT('Ctrl Pts',(3.,55.325,5.19615242270663));
#8352=CARTESIAN_POINT('Ctrl Pts',(6.,55.3625,3.46410161513776));
#8353=CARTESIAN_POINT('Ctrl Pts',(6.,55.4,0.));
#8354=CARTESIAN_POINT('Ctrl Pts',(6.,55.4375,-3.46410161513775));
#8355=CARTESIAN_POINT('Ctrl Pts',(3.,55.475,-5.19615242270663));
#8356=CARTESIAN_POINT('Ctrl Pts',(4.24230095489963E-16,55.5125,-6.92820323027551));
#8357=CARTESIAN_POINT('Ctrl Pts',(-3.,55.55,-5.19615242270663));
#8358=CARTESIAN_POINT('Ctrl Pts',(-6.,55.5875,-3.46410161513776));
#8359=CARTESIAN_POINT('Ctrl Pts',(-6.,55.625,-7.34788079488412E-16));
#8360=CARTESIAN_POINT('Ctrl Pts',(-6.,55.6625,3.46410161513775));
#8361=CARTESIAN_POINT('Ctrl Pts',(-3.,55.7,5.19615242270663));
#8362=CARTESIAN_POINT('Ctrl Pts',(-1.27269028646989E-15,55.7375,6.92820323027551));
#8363=CARTESIAN_POINT('Ctrl Pts',(3.,55.775,5.19615242270663));
#8364=CARTESIAN_POINT('Ctrl Pts',(6.,55.8125,3.46410161513776));
#8365=CARTESIAN_POINT('Ctrl Pts',(6.,55.85,0.));
#8366=CARTESIAN_POINT('Ctrl Pts',(6.,55.8875,-3.46410161513775));
#8367=CARTESIAN_POINT('Ctrl Pts',(3.,55.925,-5.19615242270663));
#8368=CARTESIAN_POINT('Ctrl Pts',(4.24230095489963E-16,55.9625,-6.92820323027551));
#8369=CARTESIAN_POINT('Ctrl Pts',(-3.,56.,-5.19615242270663));
#8370=CARTESIAN_POINT('Ctrl Pts',(-6.,56.0375,-3.46410161513776));
#8371=CARTESIAN_POINT('Ctrl Pts',(-6.,56.075,-7.34788079488412E-16));
#8372=CARTESIAN_POINT('Ctrl Pts',(-6.,56.1125,3.46410161513775));
#8373=CARTESIAN_POINT('Ctrl Pts',(-3.,56.15,5.19615242270663));
#8374=CARTESIAN_POINT('Ctrl Pts',(-1.27269028646989E-15,56.1875,6.92820323027551));
#8375=CARTESIAN_POINT('Ctrl Pts',(3.,56.225,5.19615242270663));
#8376=CARTESIAN_POINT('Ctrl Pts',(6.,56.2625,3.46410161513776));
#8377=CARTESIAN_POINT('Ctrl Pts',(6.,56.3,0.));
#8378=CARTESIAN_POINT('Ctrl Pts',(6.,56.3375,-3.46410161513775));
#8379=CARTESIAN_POINT('Ctrl Pts',(3.,56.375,-5.19615242270663));
#8380=CARTESIAN_POINT('Ctrl Pts',(4.24230095489963E-16,56.4125,-6.92820323027551));
#8381=CARTESIAN_POINT('Ctrl Pts',(-3.,56.45,-5.19615242270663));
#8382=CARTESIAN_POINT('Ctrl Pts',(-6.,56.4875,-3.46410161513776));
#8383=CARTESIAN_POINT('Ctrl Pts',(-6.,56.525,-7.34788079488412E-16));
#8384=CARTESIAN_POINT('Ctrl Pts',(-6.,56.5625,3.46410161513775));
#8385=CARTESIAN_POINT('Ctrl Pts',(-3.,56.6,5.19615242270663));
#8386=CARTESIAN_POINT('Ctrl Pts',(-1.27269028646989E-15,56.6375,6.92820323027551));
#8387=CARTESIAN_POINT('Ctrl Pts',(3.,56.675,5.19615242270663));
#8388=CARTESIAN_POINT('Ctrl Pts',(6.,56.7125,3.46410161513776));
#8389=CARTESIAN_POINT('Ctrl Pts',(6.,56.75,0.));
#8390=CARTESIAN_POINT('Ctrl Pts',(6.,56.7875,-3.46410161513775));
#8391=CARTESIAN_POINT('Ctrl Pts',(3.,56.825,-5.19615242270663));
#8392=CARTESIAN_POINT('Ctrl Pts',(4.24230095489963E-16,56.8625,-6.92820323027551));
#8393=CARTESIAN_POINT('Ctrl Pts',(-3.,56.9,-5.19615242270663));
#8394=CARTESIAN_POINT('Ctrl Pts',(-6.,56.9375,-3.46410161513776));
#8395=CARTESIAN_POINT('Ctrl Pts',(-6.,56.975,-7.34788079488412E-16));
#8396=CARTESIAN_POINT('Ctrl Pts',(-6.,57.0125,3.46410161513775));
#8397=CARTESIAN_POINT('Ctrl Pts',(-3.,57.05,5.19615242270663));
#8398=CARTESIAN_POINT('Ctrl Pts',(-1.27269028646989E-15,57.0875,6.92820323027551));
#8399=CARTESIAN_POINT('Ctrl Pts',(3.,57.125,5.19615242270663));
#8400=CARTESIAN_POINT('Ctrl Pts',(6.,57.1625,3.46410161513776));
#8401=CARTESIAN_POINT('Ctrl Pts',(6.,57.2,0.));
#8402=CARTESIAN_POINT('Ctrl Pts',(6.,57.2375,-3.46410161513775));
#8403=CARTESIAN_POINT('Ctrl Pts',(3.,57.275,-5.19615242270663));
#8404=CARTESIAN_POINT('Ctrl Pts',(4.24230095489963E-16,57.3125,-6.92820323027551));
#8405=CARTESIAN_POINT('Ctrl Pts',(-3.,57.35,-5.19615242270663));
#8406=CARTESIAN_POINT('Ctrl Pts',(-6.,57.3875,-3.46410161513776));
#8407=CARTESIAN_POINT('Ctrl Pts',(-6.,57.425,-7.34788079488412E-16));
#8408=CARTESIAN_POINT('Ctrl Pts',(-6.,57.4625,3.46410161513775));
#8409=CARTESIAN_POINT('Ctrl Pts',(-3.,57.5,5.19615242270663));
#8410=CARTESIAN_POINT('Ctrl Pts',(-1.27269028646989E-15,57.5375,6.92820323027551));
#8411=CARTESIAN_POINT('Ctrl Pts',(3.,57.575,5.19615242270663));
#8412=CARTESIAN_POINT('Ctrl Pts',(6.,57.6125,3.46410161513776));
#8413=CARTESIAN_POINT('Ctrl Pts',(6.,57.65,0.));
#8414=CARTESIAN_POINT('Ctrl Pts',(6.,57.6875,-3.46410161513775));
#8415=CARTESIAN_POINT('Ctrl Pts',(3.,57.725,-5.19615242270663));
#8416=CARTESIAN_POINT('Ctrl Pts',(4.24230095489963E-16,57.7625,-6.92820323027551));
#8417=CARTESIAN_POINT('Ctrl Pts',(-3.,57.8,-5.19615242270663));
#8418=CARTESIAN_POINT('Ctrl Pts',(-6.,57.8375,-3.46410161513776));
#8419=CARTESIAN_POINT('Ctrl Pts',(-6.,57.875,-7.34788079488412E-16));
#8420=CARTESIAN_POINT('Ctrl Pts',(-6.,57.9125,3.46410161513775));
#8421=CARTESIAN_POINT('Ctrl Pts',(-3.,57.95,5.19615242270663));
#8422=CARTESIAN_POINT('Ctrl Pts',(-1.27269028646989E-15,57.9875,6.92820323027551));
#8423=CARTESIAN_POINT('Ctrl Pts',(3.,58.025,5.19615242270663));
#8424=CARTESIAN_POINT('Ctrl Pts',(6.,58.0625,3.46410161513776));
#8425=CARTESIAN_POINT('Ctrl Pts',(6.,58.1,0.));
#8426=CARTESIAN_POINT('Ctrl Pts',(6.,58.1375,-3.46410161513775));
#8427=CARTESIAN_POINT('Ctrl Pts',(3.,58.175,-5.19615242270663));
#8428=CARTESIAN_POINT('Ctrl Pts',(4.24230095489963E-16,58.2125,-6.92820323027551));
#8429=CARTESIAN_POINT('Ctrl Pts',(-3.,58.25,-5.19615242270663));
#8430=CARTESIAN_POINT('Ctrl Pts',(-6.,58.2875,-3.46410161513776));
#8431=CARTESIAN_POINT('Ctrl Pts',(-6.,58.325,-7.34788079488412E-16));
#8432=CARTESIAN_POINT('Ctrl Pts',(-6.,58.3625,3.46410161513775));
#8433=CARTESIAN_POINT('Ctrl Pts',(-3.,58.4,5.19615242270663));
#8434=CARTESIAN_POINT('Ctrl Pts',(-1.27269028646989E-15,58.4375,6.92820323027551));
#8435=CARTESIAN_POINT('Ctrl Pts',(3.,58.475,5.19615242270663));
#8436=CARTESIAN_POINT('Ctrl Pts',(6.,58.5125,3.46410161513776));
#8437=CARTESIAN_POINT('Ctrl Pts',(6.,58.55,0.));
#8438=CARTESIAN_POINT('Ctrl Pts',(6.,58.5875,-3.46410161513775));
#8439=CARTESIAN_POINT('Ctrl Pts',(3.,58.625,-5.19615242270663));
#8440=CARTESIAN_POINT('Ctrl Pts',(4.24230095489963E-16,58.6625,-6.92820323027551));
#8441=CARTESIAN_POINT('Ctrl Pts',(-3.,58.7,-5.19615242270663));
#8442=CARTESIAN_POINT('Ctrl Pts',(-6.,58.7375,-3.46410161513776));
#8443=CARTESIAN_POINT('Ctrl Pts',(-6.,58.775,-7.34788079488412E-16));
#8444=CARTESIAN_POINT('Ctrl Pts',(-6.,58.8125,3.46410161513775));
#8445=CARTESIAN_POINT('Ctrl Pts',(-3.,58.85,5.19615242270663));
#8446=CARTESIAN_POINT('Ctrl Pts',(-1.27269028646989E-15,58.8875,6.92820323027551));
#8447=CARTESIAN_POINT('Ctrl Pts',(3.,58.925,5.19615242270663));
#8448=CARTESIAN_POINT('Ctrl Pts',(6.,58.9625,3.46410161513776));
#8449=CARTESIAN_POINT('Ctrl Pts',(6.,59.,0.));
#8450=CARTESIAN_POINT('Ctrl Pts',(6.,59.0375,-3.46410161513775));
#8451=CARTESIAN_POINT('Ctrl Pts',(3.,59.075,-5.19615242270663));
#8452=CARTESIAN_POINT('Ctrl Pts',(4.24230095489963E-16,59.1125,-6.92820323027551));
#8453=CARTESIAN_POINT('Ctrl Pts',(-3.,59.15,-5.19615242270663));
#8454=CARTESIAN_POINT('Ctrl Pts',(-6.,59.1875,-3.46410161513776));
#8455=CARTESIAN_POINT('Ctrl Pts',(-6.,59.225,-7.34788079488412E-16));
#8456=CARTESIAN_POINT('Ctrl Pts',(-6.,59.2625,3.46410161513775));
#8457=CARTESIAN_POINT('Ctrl Pts',(-3.,59.3,5.19615242270663));
#8458=CARTESIAN_POINT('Ctrl Pts',(-1.27269028646989E-15,59.3375,6.92820323027551));
#8459=CARTESIAN_POINT('Ctrl Pts',(3.,59.375,5.19615242270663));
#8460=CARTESIAN_POINT('Ctrl Pts',(6.,59.4125,3.46410161513776));
#8461=CARTESIAN_POINT('Ctrl Pts',(6.,59.45,0.));
#8462=CARTESIAN_POINT('Ctrl Pts',(6.,59.4875,-3.46410161513775));
#8463=CARTESIAN_POINT('Ctrl Pts',(3.,59.525,-5.19615242270663));
#8464=CARTESIAN_POINT('Ctrl Pts',(4.24230095489963E-16,59.5625,-6.92820323027551));
#8465=CARTESIAN_POINT('Ctrl Pts',(-3.,59.6,-5.19615242270663));
#8466=CARTESIAN_POINT('Ctrl Pts',(-6.,59.6375,-3.46410161513776));
#8467=CARTESIAN_POINT('Ctrl Pts',(-6.,59.675,-7.34788079488412E-16));
#8468=CARTESIAN_POINT('Ctrl Pts',(-6.,59.7125,3.46410161513775));
#8469=CARTESIAN_POINT('Ctrl Pts',(-3.,59.75,5.19615242270663));
#8470=CARTESIAN_POINT('Ctrl Pts',(-1.27269028646989E-15,59.7875,6.92820323027551));
#8471=CARTESIAN_POINT('Ctrl Pts',(3.,59.825,5.19615242270663));
#8472=CARTESIAN_POINT('Ctrl Pts',(6.,59.8625,3.46410161513776));
#8473=CARTESIAN_POINT('Ctrl Pts',(6.,59.9,0.));
#8474=CARTESIAN_POINT('Ctrl Pts',(6.,59.9375,-3.46410161513775));
#8475=CARTESIAN_POINT('Ctrl Pts',(3.,59.975,-5.19615242270663));
#8476=CARTESIAN_POINT('Ctrl Pts',(4.24230095489963E-16,60.0125,-6.92820323027551));
#8477=CARTESIAN_POINT('Ctrl Pts',(-3.,60.05,-5.19615242270663));
#8478=CARTESIAN_POINT('Ctrl Pts',(-6.,60.0875,-3.46410161513776));
#8479=CARTESIAN_POINT('Ctrl Pts',(-6.,60.125,-7.34788079488412E-16));
#8480=CARTESIAN_POINT('Ctrl Pts',(-6.,60.1625,3.46410161513775));
#8481=CARTESIAN_POINT('Ctrl Pts',(-3.,60.2,5.19615242270663));
#8482=CARTESIAN_POINT('Ctrl Pts',(-1.27269028646989E-15,60.2375,6.92820323027551));
#8483=CARTESIAN_POINT('Ctrl Pts',(3.,60.275,5.19615242270663));
#8484=CARTESIAN_POINT('Ctrl Pts',(6.,60.3125,3.46410161513776));
#8485=CARTESIAN_POINT('Ctrl Pts',(6.,60.35,0.));
#8486=CARTESIAN_POINT('Ctrl Pts',(6.,60.3875,-3.46410161513775));
#8487=CARTESIAN_POINT('Ctrl Pts',(3.,60.425,-5.19615242270663));
#8488=CARTESIAN_POINT('Ctrl Pts',(4.24230095489963E-16,60.4625,-6.92820323027551));
#8489=CARTESIAN_POINT('Ctrl Pts',(-3.,60.5,-5.19615242270663));
#8490=CARTESIAN_POINT('Ctrl Pts',(-6.,60.5375,-3.46410161513776));
#8491=CARTESIAN_POINT('Ctrl Pts',(-6.,60.575,-7.34788079488412E-16));
#8492=CARTESIAN_POINT('Ctrl Pts',(-6.,60.6125,3.46410161513775));
#8493=CARTESIAN_POINT('Ctrl Pts',(-3.,60.65,5.19615242270663));
#8494=CARTESIAN_POINT('Ctrl Pts',(-1.27269028646989E-15,60.6875,6.92820323027551));
#8495=CARTESIAN_POINT('Ctrl Pts',(3.,60.725,5.19615242270663));
#8496=CARTESIAN_POINT('Ctrl Pts',(6.,60.7625,3.46410161513776));
#8497=CARTESIAN_POINT('Ctrl Pts',(6.,60.8,0.));
#8498=CARTESIAN_POINT('Ctrl Pts',(6.,60.8375,-3.46410161513775));
#8499=CARTESIAN_POINT('Ctrl Pts',(3.,60.875,-5.19615242270663));
#8500=CARTESIAN_POINT('Ctrl Pts',(4.24230095489963E-16,60.9125,-6.92820323027551));
#8501=CARTESIAN_POINT('Ctrl Pts',(-3.,60.95,-5.19615242270663));
#8502=CARTESIAN_POINT('Ctrl Pts',(-6.,60.9875,-3.46410161513776));
#8503=CARTESIAN_POINT('Ctrl Pts',(-6.,61.025,-7.34788079488412E-16));
#8504=CARTESIAN_POINT('Ctrl Pts',(-6.,61.0625,3.46410161513775));
#8505=CARTESIAN_POINT('Ctrl Pts',(-3.,61.1,5.19615242270663));
#8506=CARTESIAN_POINT('Ctrl Pts',(-1.27269028646989E-15,61.1375,6.92820323027551));
#8507=CARTESIAN_POINT('Ctrl Pts',(3.,61.175,5.19615242270663));
#8508=CARTESIAN_POINT('Ctrl Pts',(6.,61.2125,3.46410161513776));
#8509=CARTESIAN_POINT('Ctrl Pts',(6.,61.25,0.));
#8510=CARTESIAN_POINT('Ctrl Pts',(6.,61.2875,-3.46410161513775));
#8511=CARTESIAN_POINT('Ctrl Pts',(3.,61.325,-5.19615242270663));
#8512=CARTESIAN_POINT('Ctrl Pts',(4.24230095489963E-16,61.3625,-6.92820323027551));
#8513=CARTESIAN_POINT('Ctrl Pts',(-3.,61.4,-5.19615242270663));
#8514=CARTESIAN_POINT('Ctrl Pts',(-6.,61.4375,-3.46410161513776));
#8515=CARTESIAN_POINT('Ctrl Pts',(-6.,61.475,-7.34788079488412E-16));
#8516=CARTESIAN_POINT('Ctrl Pts',(-6.,61.5125,3.46410161513775));
#8517=CARTESIAN_POINT('Ctrl Pts',(-3.,61.55,5.19615242270663));
#8518=CARTESIAN_POINT('Ctrl Pts',(-1.27269028646989E-15,61.5875,6.92820323027551));
#8519=CARTESIAN_POINT('Ctrl Pts',(3.,61.625,5.19615242270663));
#8520=CARTESIAN_POINT('Ctrl Pts',(6.,61.6625,3.46410161513776));
#8521=CARTESIAN_POINT('Ctrl Pts',(6.,61.7,0.));
#8522=CARTESIAN_POINT('Ctrl Pts',(6.,61.7375,-3.46410161513775));
#8523=CARTESIAN_POINT('Ctrl Pts',(3.,61.775,-5.19615242270663));
#8524=CARTESIAN_POINT('Ctrl Pts',(4.24230095489963E-16,61.8125,-6.92820323027551));
#8525=CARTESIAN_POINT('Ctrl Pts',(-3.,61.85,-5.19615242270663));
#8526=CARTESIAN_POINT('Ctrl Pts',(-6.,61.8875,-3.46410161513776));
#8527=CARTESIAN_POINT('Ctrl Pts',(-6.,61.925,-7.34788079488412E-16));
#8528=CARTESIAN_POINT('Ctrl Pts',(-6.,61.9625,3.46410161513775));
#8529=CARTESIAN_POINT('Ctrl Pts',(-3.,62.,5.19615242270663));
#8530=CARTESIAN_POINT('Ctrl Pts',(5.75643035625,50.1406249993855,0.));
#8531=CARTESIAN_POINT('Ctrl Pts',(5.75643035625,50.1781249993855,-3.32347661575227));
#8532=CARTESIAN_POINT('Ctrl Pts',(2.878215178125,50.2156249993855,-4.9852149236284));
#8533=CARTESIAN_POINT('Ctrl Pts',(4.0700849995221E-16,50.2531249993855,
-6.64695323150454));
#8534=CARTESIAN_POINT('Ctrl Pts',(-2.878215178125,50.2906249993855,-4.9852149236284));
#8535=CARTESIAN_POINT('Ctrl Pts',(-5.75643035625,50.3281249993855,-3.32347661575227));
#8536=CARTESIAN_POINT('Ctrl Pts',(-5.75643035625,50.3656249993855,-7.04959401029622E-16));
#8537=CARTESIAN_POINT('Origin',(-2.22044604925031E-15,50.1968749993855,
-2.77555756156289E-16));
#8538=CARTESIAN_POINT('Ctrl Pts',(5.75643035625,50.2531249993855,0.));
#8539=CARTESIAN_POINT('Ctrl Pts',(5.75643035625,50.2906249993855,-3.32347661575227));
#8540=CARTESIAN_POINT('Ctrl Pts',(2.878215178125,50.3281249993855,-4.9852149236284));
#8541=CARTESIAN_POINT('Ctrl Pts',(4.0700849995221E-16,50.3656249993855,
-6.64695323150454));
#8542=CARTESIAN_POINT('Ctrl Pts',(-2.878215178125,50.4031249993855,-4.9852149236284));
#8543=CARTESIAN_POINT('Ctrl Pts',(-5.75643035625,50.4406249993855,-3.32347661575227));
#8544=CARTESIAN_POINT('Ctrl Pts',(-5.75643035625,50.4781249993855,-7.04959401029622E-16));
#8545=CARTESIAN_POINT('Ctrl Pts',(6.,50.393749998771,0.));
#8546=CARTESIAN_POINT('Ctrl Pts',(6.,50.431249998771,-3.46410161513775));
#8547=CARTESIAN_POINT('Ctrl Pts',(3.,50.468749998771,-5.19615242270663));
#8548=CARTESIAN_POINT('Ctrl Pts',(4.24230095489963E-16,50.506249998771,
-6.92820323027551));
#8549=CARTESIAN_POINT('Ctrl Pts',(-3.,50.543749998771,-5.19615242270663));
#8550=CARTESIAN_POINT('Ctrl Pts',(-6.,50.581249998771,-3.46410161513776));
#8551=CARTESIAN_POINT('Ctrl Pts',(-6.,50.618749998771,-7.34788079488412E-16));
#8552=CARTESIAN_POINT('Ctrl Pts',(-6.,50.656249998771,3.46410161513775));
#8553=CARTESIAN_POINT('Ctrl Pts',(-3.,50.693749998771,5.19615242270663));
#8554=CARTESIAN_POINT('Ctrl Pts',(-1.27269028646989E-15,50.731249998771,
6.92820323027551));
#8555=CARTESIAN_POINT('Ctrl Pts',(3.,50.768749998771,5.19615242270663));
#8556=CARTESIAN_POINT('Ctrl Pts',(6.,50.806249998771,3.46410161513776));
#8557=CARTESIAN_POINT('Ctrl Pts',(6.,50.843749998771,0.));
#8558=CARTESIAN_POINT('Ctrl Pts',(6.,50.881249998771,-3.46410161513775));
#8559=CARTESIAN_POINT('Ctrl Pts',(3.,50.918749998771,-5.19615242270663));
#8560=CARTESIAN_POINT('Ctrl Pts',(4.24230095489963E-16,50.956249998771,
-6.92820323027551));
#8561=CARTESIAN_POINT('Ctrl Pts',(-3.,50.993749998771,-5.19615242270663));
#8562=CARTESIAN_POINT('Ctrl Pts',(-6.,51.031249998771,-3.46410161513776));
#8563=CARTESIAN_POINT('Ctrl Pts',(-6.,51.068749998771,-7.34788079488412E-16));
#8564=CARTESIAN_POINT('Ctrl Pts',(-6.,51.106249998771,3.46410161513775));
#8565=CARTESIAN_POINT('Ctrl Pts',(-3.,51.143749998771,5.19615242270663));
#8566=CARTESIAN_POINT('Ctrl Pts',(-1.27269028646989E-15,51.181249998771,
6.92820323027551));
#8567=CARTESIAN_POINT('Ctrl Pts',(3.,51.218749998771,5.19615242270663));
#8568=CARTESIAN_POINT('Ctrl Pts',(6.,51.256249998771,3.46410161513776));
#8569=CARTESIAN_POINT('Ctrl Pts',(6.,51.293749998771,0.));
#8570=CARTESIAN_POINT('Ctrl Pts',(6.,51.331249998771,-3.46410161513775));
#8571=CARTESIAN_POINT('Ctrl Pts',(3.,51.368749998771,-5.19615242270663));
#8572=CARTESIAN_POINT('Ctrl Pts',(4.24230095489963E-16,51.406249998771,
-6.92820323027551));
#8573=CARTESIAN_POINT('Ctrl Pts',(-3.,51.443749998771,-5.19615242270663));
#8574=CARTESIAN_POINT('Ctrl Pts',(-6.,51.481249998771,-3.46410161513776));
#8575=CARTESIAN_POINT('Ctrl Pts',(-6.,51.518749998771,-7.34788079488412E-16));
#8576=CARTESIAN_POINT('Ctrl Pts',(-6.,51.556249998771,3.46410161513775));
#8577=CARTESIAN_POINT('Ctrl Pts',(-3.,51.593749998771,5.19615242270663));
#8578=CARTESIAN_POINT('Ctrl Pts',(-1.27269028646989E-15,51.631249998771,
6.92820323027551));
#8579=CARTESIAN_POINT('Ctrl Pts',(3.,51.668749998771,5.19615242270663));
#8580=CARTESIAN_POINT('Ctrl Pts',(6.,51.706249998771,3.46410161513776));
#8581=CARTESIAN_POINT('Ctrl Pts',(6.,51.743749998771,0.));
#8582=CARTESIAN_POINT('Ctrl Pts',(6.,51.781249998771,-3.46410161513775));
#8583=CARTESIAN_POINT('Ctrl Pts',(3.,51.818749998771,-5.19615242270663));
#8584=CARTESIAN_POINT('Ctrl Pts',(4.24230095489963E-16,51.856249998771,
-6.92820323027551));
#8585=CARTESIAN_POINT('Ctrl Pts',(-3.,51.893749998771,-5.19615242270663));
#8586=CARTESIAN_POINT('Ctrl Pts',(-6.,51.931249998771,-3.46410161513776));
#8587=CARTESIAN_POINT('Ctrl Pts',(-6.,51.968749998771,-7.34788079488412E-16));
#8588=CARTESIAN_POINT('Ctrl Pts',(-6.,52.006249998771,3.46410161513775));
#8589=CARTESIAN_POINT('Ctrl Pts',(-3.,52.043749998771,5.19615242270663));
#8590=CARTESIAN_POINT('Ctrl Pts',(-1.27269028646989E-15,52.081249998771,
6.92820323027551));
#8591=CARTESIAN_POINT('Ctrl Pts',(3.,52.118749998771,5.19615242270663));
#8592=CARTESIAN_POINT('Ctrl Pts',(6.,52.156249998771,3.46410161513776));
#8593=CARTESIAN_POINT('Ctrl Pts',(6.,52.193749998771,0.));
#8594=CARTESIAN_POINT('Ctrl Pts',(6.,52.231249998771,-3.46410161513775));
#8595=CARTESIAN_POINT('Ctrl Pts',(3.,52.268749998771,-5.19615242270663));
#8596=CARTESIAN_POINT('Ctrl Pts',(4.24230095489963E-16,52.306249998771,
-6.92820323027551));
#8597=CARTESIAN_POINT('Ctrl Pts',(-3.,52.343749998771,-5.19615242270663));
#8598=CARTESIAN_POINT('Ctrl Pts',(-6.,52.381249998771,-3.46410161513776));
#8599=CARTESIAN_POINT('Ctrl Pts',(-6.,52.418749998771,-7.34788079488412E-16));
#8600=CARTESIAN_POINT('Ctrl Pts',(-6.,52.456249998771,3.46410161513775));
#8601=CARTESIAN_POINT('Ctrl Pts',(-3.,52.493749998771,5.19615242270663));
#8602=CARTESIAN_POINT('Ctrl Pts',(-1.27269028646989E-15,52.531249998771,
6.92820323027551));
#8603=CARTESIAN_POINT('Ctrl Pts',(3.,52.568749998771,5.19615242270663));
#8604=CARTESIAN_POINT('Ctrl Pts',(6.,52.606249998771,3.46410161513776));
#8605=CARTESIAN_POINT('Ctrl Pts',(6.,52.643749998771,0.));
#8606=CARTESIAN_POINT('Ctrl Pts',(6.,52.681249998771,-3.46410161513775));
#8607=CARTESIAN_POINT('Ctrl Pts',(3.,52.718749998771,-5.19615242270663));
#8608=CARTESIAN_POINT('Ctrl Pts',(4.24230095489963E-16,52.756249998771,
-6.92820323027551));
#8609=CARTESIAN_POINT('Ctrl Pts',(-3.,52.793749998771,-5.19615242270663));
#8610=CARTESIAN_POINT('Ctrl Pts',(-6.,52.831249998771,-3.46410161513776));
#8611=CARTESIAN_POINT('Ctrl Pts',(-6.,52.868749998771,-7.34788079488412E-16));
#8612=CARTESIAN_POINT('Ctrl Pts',(-6.,52.906249998771,3.46410161513775));
#8613=CARTESIAN_POINT('Ctrl Pts',(-3.,52.943749998771,5.19615242270663));
#8614=CARTESIAN_POINT('Ctrl Pts',(-1.27269028646989E-15,52.981249998771,
6.92820323027551));
#8615=CARTESIAN_POINT('Ctrl Pts',(3.,53.018749998771,5.19615242270663));
#8616=CARTESIAN_POINT('Ctrl Pts',(6.,53.056249998771,3.46410161513776));
#8617=CARTESIAN_POINT('Ctrl Pts',(6.,53.093749998771,0.));
#8618=CARTESIAN_POINT('Ctrl Pts',(6.,53.131249998771,-3.46410161513775));
#8619=CARTESIAN_POINT('Ctrl Pts',(3.,53.168749998771,-5.19615242270663));
#8620=CARTESIAN_POINT('Ctrl Pts',(4.24230095489963E-16,53.206249998771,
-6.92820323027551));
#8621=CARTESIAN_POINT('Ctrl Pts',(-3.,53.243749998771,-5.19615242270663));
#8622=CARTESIAN_POINT('Ctrl Pts',(-6.,53.281249998771,-3.46410161513776));
#8623=CARTESIAN_POINT('Ctrl Pts',(-6.,53.318749998771,-7.34788079488412E-16));
#8624=CARTESIAN_POINT('Ctrl Pts',(-6.,53.356249998771,3.46410161513775));
#8625=CARTESIAN_POINT('Ctrl Pts',(-3.,53.393749998771,5.19615242270663));
#8626=CARTESIAN_POINT('Ctrl Pts',(-1.27269028646989E-15,53.431249998771,
6.92820323027551));
#8627=CARTESIAN_POINT('Ctrl Pts',(3.,53.468749998771,5.19615242270663));
#8628=CARTESIAN_POINT('Ctrl Pts',(6.,53.506249998771,3.46410161513776));
#8629=CARTESIAN_POINT('Ctrl Pts',(6.,53.543749998771,0.));
#8630=CARTESIAN_POINT('Ctrl Pts',(6.,53.581249998771,-3.46410161513775));
#8631=CARTESIAN_POINT('Ctrl Pts',(3.,53.618749998771,-5.19615242270663));
#8632=CARTESIAN_POINT('Ctrl Pts',(4.24230095489963E-16,53.656249998771,
-6.92820323027551));
#8633=CARTESIAN_POINT('Ctrl Pts',(-3.,53.693749998771,-5.19615242270663));
#8634=CARTESIAN_POINT('Ctrl Pts',(-6.,53.731249998771,-3.46410161513776));
#8635=CARTESIAN_POINT('Ctrl Pts',(-6.,53.768749998771,-7.34788079488412E-16));
#8636=CARTESIAN_POINT('Ctrl Pts',(-6.,53.806249998771,3.46410161513775));
#8637=CARTESIAN_POINT('Ctrl Pts',(-3.,53.843749998771,5.19615242270663));
#8638=CARTESIAN_POINT('Ctrl Pts',(-1.27269028646989E-15,53.881249998771,
6.92820323027551));
#8639=CARTESIAN_POINT('Ctrl Pts',(3.,53.918749998771,5.19615242270663));
#8640=CARTESIAN_POINT('Ctrl Pts',(6.,53.956249998771,3.46410161513776));
#8641=CARTESIAN_POINT('Ctrl Pts',(6.,53.993749998771,0.));
#8642=CARTESIAN_POINT('Ctrl Pts',(6.,54.031249998771,-3.46410161513775));
#8643=CARTESIAN_POINT('Ctrl Pts',(3.,54.068749998771,-5.19615242270663));
#8644=CARTESIAN_POINT('Ctrl Pts',(4.24230095489963E-16,54.106249998771,
-6.92820323027551));
#8645=CARTESIAN_POINT('Ctrl Pts',(-3.,54.143749998771,-5.19615242270663));
#8646=CARTESIAN_POINT('Ctrl Pts',(-6.,54.181249998771,-3.46410161513776));
#8647=CARTESIAN_POINT('Ctrl Pts',(-6.,54.218749998771,-7.34788079488412E-16));
#8648=CARTESIAN_POINT('Ctrl Pts',(-6.,54.256249998771,3.46410161513775));
#8649=CARTESIAN_POINT('Ctrl Pts',(-3.,54.293749998771,5.19615242270663));
#8650=CARTESIAN_POINT('Ctrl Pts',(-1.27269028646989E-15,54.331249998771,
6.92820323027551));
#8651=CARTESIAN_POINT('Ctrl Pts',(3.,54.368749998771,5.19615242270663));
#8652=CARTESIAN_POINT('Ctrl Pts',(6.,54.406249998771,3.46410161513776));
#8653=CARTESIAN_POINT('Ctrl Pts',(6.,54.443749998771,0.));
#8654=CARTESIAN_POINT('Ctrl Pts',(6.,54.481249998771,-3.46410161513775));
#8655=CARTESIAN_POINT('Ctrl Pts',(3.,54.518749998771,-5.19615242270663));
#8656=CARTESIAN_POINT('Ctrl Pts',(4.24230095489963E-16,54.556249998771,
-6.92820323027551));
#8657=CARTESIAN_POINT('Ctrl Pts',(-3.,54.593749998771,-5.19615242270663));
#8658=CARTESIAN_POINT('Ctrl Pts',(-6.,54.631249998771,-3.46410161513776));
#8659=CARTESIAN_POINT('Ctrl Pts',(-6.,54.668749998771,-7.34788079488412E-16));
#8660=CARTESIAN_POINT('Ctrl Pts',(-6.,54.706249998771,3.46410161513775));
#8661=CARTESIAN_POINT('Ctrl Pts',(-3.,54.743749998771,5.19615242270663));
#8662=CARTESIAN_POINT('Ctrl Pts',(-1.27269028646989E-15,54.781249998771,
6.92820323027551));
#8663=CARTESIAN_POINT('Ctrl Pts',(3.,54.818749998771,5.19615242270663));
#8664=CARTESIAN_POINT('Ctrl Pts',(6.,54.856249998771,3.46410161513776));
#8665=CARTESIAN_POINT('Ctrl Pts',(6.,54.893749998771,0.));
#8666=CARTESIAN_POINT('Ctrl Pts',(6.,54.931249998771,-3.46410161513775));
#8667=CARTESIAN_POINT('Ctrl Pts',(3.,54.968749998771,-5.19615242270663));
#8668=CARTESIAN_POINT('Ctrl Pts',(4.24230095489963E-16,55.006249998771,
-6.92820323027551));
#8669=CARTESIAN_POINT('Ctrl Pts',(-3.,55.043749998771,-5.19615242270663));
#8670=CARTESIAN_POINT('Ctrl Pts',(-6.,55.081249998771,-3.46410161513776));
#8671=CARTESIAN_POINT('Ctrl Pts',(-6.,55.118749998771,-7.34788079488412E-16));
#8672=CARTESIAN_POINT('Ctrl Pts',(-6.,55.156249998771,3.46410161513775));
#8673=CARTESIAN_POINT('Ctrl Pts',(-3.,55.193749998771,5.19615242270663));
#8674=CARTESIAN_POINT('Ctrl Pts',(-1.27269028646989E-15,55.231249998771,
6.92820323027551));
#8675=CARTESIAN_POINT('Ctrl Pts',(3.,55.268749998771,5.19615242270663));
#8676=CARTESIAN_POINT('Ctrl Pts',(6.,55.306249998771,3.46410161513776));
#8677=CARTESIAN_POINT('Ctrl Pts',(6.,55.343749998771,0.));
#8678=CARTESIAN_POINT('Ctrl Pts',(6.,55.381249998771,-3.46410161513775));
#8679=CARTESIAN_POINT('Ctrl Pts',(3.,55.418749998771,-5.19615242270663));
#8680=CARTESIAN_POINT('Ctrl Pts',(4.24230095489963E-16,55.456249998771,
-6.92820323027551));
#8681=CARTESIAN_POINT('Ctrl Pts',(-3.,55.493749998771,-5.19615242270663));
#8682=CARTESIAN_POINT('Ctrl Pts',(-6.,55.531249998771,-3.46410161513776));
#8683=CARTESIAN_POINT('Ctrl Pts',(-6.,55.568749998771,-7.34788079488412E-16));
#8684=CARTESIAN_POINT('Ctrl Pts',(-6.,55.606249998771,3.46410161513775));
#8685=CARTESIAN_POINT('Ctrl Pts',(-3.,55.643749998771,5.19615242270663));
#8686=CARTESIAN_POINT('Ctrl Pts',(-1.27269028646989E-15,55.681249998771,
6.92820323027551));
#8687=CARTESIAN_POINT('Ctrl Pts',(3.,55.718749998771,5.19615242270663));
#8688=CARTESIAN_POINT('Ctrl Pts',(6.,55.756249998771,3.46410161513776));
#8689=CARTESIAN_POINT('Ctrl Pts',(6.,55.793749998771,0.));
#8690=CARTESIAN_POINT('Ctrl Pts',(6.,55.831249998771,-3.46410161513775));
#8691=CARTESIAN_POINT('Ctrl Pts',(3.,55.868749998771,-5.19615242270663));
#8692=CARTESIAN_POINT('Ctrl Pts',(4.24230095489963E-16,55.906249998771,
-6.92820323027551));
#8693=CARTESIAN_POINT('Ctrl Pts',(-3.,55.943749998771,-5.19615242270663));
#8694=CARTESIAN_POINT('Ctrl Pts',(-6.,55.981249998771,-3.46410161513776));
#8695=CARTESIAN_POINT('Ctrl Pts',(-6.,56.018749998771,-7.34788079488412E-16));
#8696=CARTESIAN_POINT('Ctrl Pts',(-6.,56.056249998771,3.46410161513775));
#8697=CARTESIAN_POINT('Ctrl Pts',(-3.,56.093749998771,5.19615242270663));
#8698=CARTESIAN_POINT('Ctrl Pts',(-1.27269028646989E-15,56.1312499987709,
6.92820323027551));
#8699=CARTESIAN_POINT('Ctrl Pts',(3.,56.168749998771,5.19615242270663));
#8700=CARTESIAN_POINT('Ctrl Pts',(6.,56.206249998771,3.46410161513776));
#8701=CARTESIAN_POINT('Ctrl Pts',(6.,56.243749998771,0.));
#8702=CARTESIAN_POINT('Ctrl Pts',(6.,56.281249998771,-3.46410161513775));
#8703=CARTESIAN_POINT('Ctrl Pts',(3.,56.318749998771,-5.19615242270663));
#8704=CARTESIAN_POINT('Ctrl Pts',(4.24230095489963E-16,56.3562499987709,
-6.92820323027551));
#8705=CARTESIAN_POINT('Ctrl Pts',(-3.,56.393749998771,-5.19615242270663));
#8706=CARTESIAN_POINT('Ctrl Pts',(-6.,56.431249998771,-3.46410161513776));
#8707=CARTESIAN_POINT('Ctrl Pts',(-6.,56.468749998771,-7.34788079488412E-16));
#8708=CARTESIAN_POINT('Ctrl Pts',(-6.,56.506249998771,3.46410161513775));
#8709=CARTESIAN_POINT('Ctrl Pts',(-3.,56.543749998771,5.19615242270663));
#8710=CARTESIAN_POINT('Ctrl Pts',(-1.27269028646989E-15,56.581249998771,
6.92820323027551));
#8711=CARTESIAN_POINT('Ctrl Pts',(3.,56.618749998771,5.19615242270663));
#8712=CARTESIAN_POINT('Ctrl Pts',(6.,56.656249998771,3.46410161513776));
#8713=CARTESIAN_POINT('Ctrl Pts',(6.,56.693749998771,0.));
#8714=CARTESIAN_POINT('Ctrl Pts',(6.,56.731249998771,-3.46410161513775));
#8715=CARTESIAN_POINT('Ctrl Pts',(3.,56.768749998771,-5.19615242270663));
#8716=CARTESIAN_POINT('Ctrl Pts',(4.24230095489963E-16,56.806249998771,
-6.92820323027551));
#8717=CARTESIAN_POINT('Ctrl Pts',(-3.,56.843749998771,-5.19615242270663));
#8718=CARTESIAN_POINT('Ctrl Pts',(-6.,56.881249998771,-3.46410161513776));
#8719=CARTESIAN_POINT('Ctrl Pts',(-6.,56.918749998771,-7.34788079488412E-16));
#8720=CARTESIAN_POINT('Ctrl Pts',(-6.,56.956249998771,3.46410161513775));
#8721=CARTESIAN_POINT('Ctrl Pts',(-3.,56.993749998771,5.19615242270663));
#8722=CARTESIAN_POINT('Ctrl Pts',(-1.27269028646989E-15,57.031249998771,
6.92820323027551));
#8723=CARTESIAN_POINT('Ctrl Pts',(3.,57.068749998771,5.19615242270663));
#8724=CARTESIAN_POINT('Ctrl Pts',(6.,57.106249998771,3.46410161513776));
#8725=CARTESIAN_POINT('Ctrl Pts',(6.,57.143749998771,0.));
#8726=CARTESIAN_POINT('Ctrl Pts',(6.,57.181249998771,-3.46410161513775));
#8727=CARTESIAN_POINT('Ctrl Pts',(3.,57.218749998771,-5.19615242270663));
#8728=CARTESIAN_POINT('Ctrl Pts',(4.24230095489963E-16,57.256249998771,
-6.92820323027551));
#8729=CARTESIAN_POINT('Ctrl Pts',(-3.,57.293749998771,-5.19615242270663));
#8730=CARTESIAN_POINT('Ctrl Pts',(-6.,57.331249998771,-3.46410161513776));
#8731=CARTESIAN_POINT('Ctrl Pts',(-6.,57.368749998771,-7.34788079488412E-16));
#8732=CARTESIAN_POINT('Ctrl Pts',(-6.,57.406249998771,3.46410161513775));
#8733=CARTESIAN_POINT('Ctrl Pts',(-3.,57.443749998771,5.19615242270663));
#8734=CARTESIAN_POINT('Ctrl Pts',(-1.27269028646989E-15,57.481249998771,
6.92820323027551));
#8735=CARTESIAN_POINT('Ctrl Pts',(3.,57.518749998771,5.19615242270663));
#8736=CARTESIAN_POINT('Ctrl Pts',(6.,57.556249998771,3.46410161513776));
#8737=CARTESIAN_POINT('Ctrl Pts',(6.,57.593749998771,0.));
#8738=CARTESIAN_POINT('Ctrl Pts',(6.,57.631249998771,-3.46410161513775));
#8739=CARTESIAN_POINT('Ctrl Pts',(3.,57.668749998771,-5.19615242270663));
#8740=CARTESIAN_POINT('Ctrl Pts',(4.24230095489963E-16,57.706249998771,
-6.92820323027551));
#8741=CARTESIAN_POINT('Ctrl Pts',(-3.,57.743749998771,-5.19615242270663));
#8742=CARTESIAN_POINT('Ctrl Pts',(-6.,57.781249998771,-3.46410161513776));
#8743=CARTESIAN_POINT('Ctrl Pts',(-6.,57.818749998771,-7.34788079488412E-16));
#8744=CARTESIAN_POINT('Ctrl Pts',(-6.,57.8562499987709,3.46410161513775));
#8745=CARTESIAN_POINT('Ctrl Pts',(-3.,57.893749998771,5.19615242270663));
#8746=CARTESIAN_POINT('Ctrl Pts',(-1.27269028646989E-15,57.931249998771,
6.92820323027551));
#8747=CARTESIAN_POINT('Ctrl Pts',(3.,57.968749998771,5.19615242270663));
#8748=CARTESIAN_POINT('Ctrl Pts',(6.,58.0062499987709,3.46410161513776));
#8749=CARTESIAN_POINT('Ctrl Pts',(6.,58.043749998771,0.));
#8750=CARTESIAN_POINT('Ctrl Pts',(6.,58.081249998771,-3.46410161513775));
#8751=CARTESIAN_POINT('Ctrl Pts',(3.,58.118749998771,-5.19615242270663));
#8752=CARTESIAN_POINT('Ctrl Pts',(4.24230095489963E-16,58.156249998771,
-6.92820323027551));
#8753=CARTESIAN_POINT('Ctrl Pts',(-3.,58.193749998771,-5.19615242270663));
#8754=CARTESIAN_POINT('Ctrl Pts',(-6.,58.231249998771,-3.46410161513776));
#8755=CARTESIAN_POINT('Ctrl Pts',(-6.,58.268749998771,-7.34788079488412E-16));
#8756=CARTESIAN_POINT('Ctrl Pts',(-6.,58.306249998771,3.46410161513775));
#8757=CARTESIAN_POINT('Ctrl Pts',(-3.,58.343749998771,5.19615242270663));
#8758=CARTESIAN_POINT('Ctrl Pts',(-1.27269028646989E-15,58.381249998771,
6.92820323027551));
#8759=CARTESIAN_POINT('Ctrl Pts',(3.,58.418749998771,5.19615242270663));
#8760=CARTESIAN_POINT('Ctrl Pts',(6.,58.456249998771,3.46410161513776));
#8761=CARTESIAN_POINT('Ctrl Pts',(6.,58.493749998771,0.));
#8762=CARTESIAN_POINT('Ctrl Pts',(6.,58.531249998771,-3.46410161513775));
#8763=CARTESIAN_POINT('Ctrl Pts',(3.,58.568749998771,-5.19615242270663));
#8764=CARTESIAN_POINT('Ctrl Pts',(4.24230095489963E-16,58.606249998771,
-6.92820323027551));
#8765=CARTESIAN_POINT('Ctrl Pts',(-3.,58.643749998771,-5.19615242270663));
#8766=CARTESIAN_POINT('Ctrl Pts',(-6.,58.681249998771,-3.46410161513776));
#8767=CARTESIAN_POINT('Ctrl Pts',(-6.,58.718749998771,-7.34788079488412E-16));
#8768=CARTESIAN_POINT('Ctrl Pts',(-6.,58.756249998771,3.46410161513775));
#8769=CARTESIAN_POINT('Ctrl Pts',(-3.,58.793749998771,5.19615242270663));
#8770=CARTESIAN_POINT('Ctrl Pts',(-1.27269028646989E-15,58.831249998771,
6.92820323027551));
#8771=CARTESIAN_POINT('Ctrl Pts',(3.,58.868749998771,5.19615242270663));
#8772=CARTESIAN_POINT('Ctrl Pts',(6.,58.906249998771,3.46410161513776));
#8773=CARTESIAN_POINT('Ctrl Pts',(6.,58.943749998771,0.));
#8774=CARTESIAN_POINT('Ctrl Pts',(6.,58.981249998771,-3.46410161513775));
#8775=CARTESIAN_POINT('Ctrl Pts',(3.,59.018749998771,-5.19615242270663));
#8776=CARTESIAN_POINT('Ctrl Pts',(4.24230095489963E-16,59.056249998771,
-6.92820323027551));
#8777=CARTESIAN_POINT('Ctrl Pts',(-3.,59.093749998771,-5.19615242270663));
#8778=CARTESIAN_POINT('Ctrl Pts',(-6.,59.1312499987709,-3.46410161513776));
#8779=CARTESIAN_POINT('Ctrl Pts',(-6.,59.168749998771,-7.34788079488412E-16));
#8780=CARTESIAN_POINT('Ctrl Pts',(-6.,59.206249998771,3.46410161513775));
#8781=CARTESIAN_POINT('Ctrl Pts',(-3.,59.243749998771,5.19615242270663));
#8782=CARTESIAN_POINT('Ctrl Pts',(-1.27269028646989E-15,59.281249998771,
6.92820323027551));
#8783=CARTESIAN_POINT('Ctrl Pts',(3.,59.318749998771,5.19615242270663));
#8784=CARTESIAN_POINT('Ctrl Pts',(6.,59.356249998771,3.46410161513776));
#8785=CARTESIAN_POINT('Ctrl Pts',(6.,59.393749998771,0.));
#8786=CARTESIAN_POINT('Ctrl Pts',(6.,59.431249998771,-3.46410161513775));
#8787=CARTESIAN_POINT('Ctrl Pts',(3.,59.468749998771,-5.19615242270663));
#8788=CARTESIAN_POINT('Ctrl Pts',(4.24230095489963E-16,59.506249998771,
-6.92820323027551));
#8789=CARTESIAN_POINT('Ctrl Pts',(-3.,59.543749998771,-5.19615242270663));
#8790=CARTESIAN_POINT('Ctrl Pts',(-6.,59.581249998771,-3.46410161513776));
#8791=CARTESIAN_POINT('Ctrl Pts',(-6.,59.618749998771,-7.34788079488412E-16));
#8792=CARTESIAN_POINT('Ctrl Pts',(-6.,59.656249998771,3.46410161513775));
#8793=CARTESIAN_POINT('Ctrl Pts',(-3.,59.693749998771,5.19615242270663));
#8794=CARTESIAN_POINT('Ctrl Pts',(-1.27269028646989E-15,59.731249998771,
6.92820323027551));
#8795=CARTESIAN_POINT('Ctrl Pts',(3.,59.768749998771,5.19615242270663));
#8796=CARTESIAN_POINT('Ctrl Pts',(6.,59.806249998771,3.46410161513776));
#8797=CARTESIAN_POINT('Ctrl Pts',(6.,59.843749998771,0.));
#8798=CARTESIAN_POINT('Ctrl Pts',(6.,59.881249998771,-3.46410161513775));
#8799=CARTESIAN_POINT('Ctrl Pts',(3.,59.918749998771,-5.19615242270663));
#8800=CARTESIAN_POINT('Ctrl Pts',(4.24230095489963E-16,59.956249998771,
-6.92820323027551));
#8801=CARTESIAN_POINT('Ctrl Pts',(-3.,59.993749998771,-5.19615242270663));
#8802=CARTESIAN_POINT('Ctrl Pts',(-6.,60.031249998771,-3.46410161513776));
#8803=CARTESIAN_POINT('Ctrl Pts',(-6.,60.068749998771,-7.34788079488412E-16));
#8804=CARTESIAN_POINT('Ctrl Pts',(-6.,60.106249998771,3.46410161513775));
#8805=CARTESIAN_POINT('Ctrl Pts',(-3.,60.143749998771,5.19615242270663));
#8806=CARTESIAN_POINT('Ctrl Pts',(-1.27269028646989E-15,60.181249998771,
6.92820323027551));
#8807=CARTESIAN_POINT('Ctrl Pts',(3.,60.218749998771,5.19615242270663));
#8808=CARTESIAN_POINT('Ctrl Pts',(6.,60.256249998771,3.46410161513776));
#8809=CARTESIAN_POINT('Ctrl Pts',(6.,60.293749998771,0.));
#8810=CARTESIAN_POINT('Ctrl Pts',(6.,60.331249998771,-3.46410161513775));
#8811=CARTESIAN_POINT('Ctrl Pts',(3.,60.368749998771,-5.19615242270663));
#8812=CARTESIAN_POINT('Ctrl Pts',(4.24230095489963E-16,60.406249998771,
-6.92820323027551));
#8813=CARTESIAN_POINT('Ctrl Pts',(-3.,60.443749998771,-5.19615242270663));
#8814=CARTESIAN_POINT('Ctrl Pts',(-6.,60.481249998771,-3.46410161513776));
#8815=CARTESIAN_POINT('Ctrl Pts',(-6.,60.518749998771,-7.34788079488412E-16));
#8816=CARTESIAN_POINT('Ctrl Pts',(-6.,60.556249998771,3.46410161513775));
#8817=CARTESIAN_POINT('Ctrl Pts',(-3.,60.593749998771,5.19615242270663));
#8818=CARTESIAN_POINT('Ctrl Pts',(-1.27269028646989E-15,60.631249998771,
6.92820323027551));
#8819=CARTESIAN_POINT('Ctrl Pts',(3.,60.668749998771,5.19615242270663));
#8820=CARTESIAN_POINT('Ctrl Pts',(6.,60.706249998771,3.46410161513776));
#8821=CARTESIAN_POINT('Ctrl Pts',(6.,60.743749998771,0.));
#8822=CARTESIAN_POINT('Ctrl Pts',(6.,60.781249998771,-3.46410161513775));
#8823=CARTESIAN_POINT('Ctrl Pts',(3.,60.818749998771,-5.19615242270663));
#8824=CARTESIAN_POINT('Ctrl Pts',(4.24230095489963E-16,60.856249998771,
-6.92820323027551));
#8825=CARTESIAN_POINT('Ctrl Pts',(-3.,60.893749998771,-5.19615242270663));
#8826=CARTESIAN_POINT('Ctrl Pts',(-6.,60.931249998771,-3.46410161513776));
#8827=CARTESIAN_POINT('Ctrl Pts',(-6.,60.968749998771,-7.34788079488412E-16));
#8828=CARTESIAN_POINT('Ctrl Pts',(-6.,61.0062499987709,3.46410161513775));
#8829=CARTESIAN_POINT('Ctrl Pts',(-3.,61.043749998771,5.19615242270663));
#8830=CARTESIAN_POINT('Ctrl Pts',(-1.27269028646989E-15,61.081249998771,
6.92820323027551));
#8831=CARTESIAN_POINT('Ctrl Pts',(3.,61.118749998771,5.19615242270663));
#8832=CARTESIAN_POINT('Ctrl Pts',(6.,61.156249998771,3.46410161513776));
#8833=CARTESIAN_POINT('Ctrl Pts',(6.,61.193749998771,0.));
#8834=CARTESIAN_POINT('Ctrl Pts',(6.,61.231249998771,-3.46410161513775));
#8835=CARTESIAN_POINT('Ctrl Pts',(3.,61.268749998771,-5.19615242270663));
#8836=CARTESIAN_POINT('Ctrl Pts',(4.24230095489963E-16,61.306249998771,
-6.92820323027551));
#8837=CARTESIAN_POINT('Ctrl Pts',(-3.,61.343749998771,-5.19615242270663));
#8838=CARTESIAN_POINT('Ctrl Pts',(-6.,61.381249998771,-3.46410161513776));
#8839=CARTESIAN_POINT('Ctrl Pts',(-6.,61.418749998771,-7.34788079488412E-16));
#8840=CARTESIAN_POINT('Ctrl Pts',(-6.,61.456249998771,3.46410161513775));
#8841=CARTESIAN_POINT('Ctrl Pts',(-3.,61.493749998771,5.19615242270663));
#8842=CARTESIAN_POINT('Ctrl Pts',(-1.27269028646989E-15,61.531249998771,
6.92820323027551));
#8843=CARTESIAN_POINT('Ctrl Pts',(3.,61.568749998771,5.19615242270663));
#8844=CARTESIAN_POINT('Ctrl Pts',(6.,61.606249998771,3.46410161513776));
#8845=CARTESIAN_POINT('Ctrl Pts',(6.,61.643749998771,0.));
#8846=CARTESIAN_POINT('Ctrl Pts',(6.,61.681249998771,-3.46410161513775));
#8847=CARTESIAN_POINT('Ctrl Pts',(3.,61.718749998771,-5.19615242270663));
#8848=CARTESIAN_POINT('Ctrl Pts',(4.24230095489963E-16,61.756249998771,
-6.92820323027551));
#8849=CARTESIAN_POINT('Ctrl Pts',(-3.,61.793749998771,-5.19615242270663));
#8850=CARTESIAN_POINT('Ctrl Pts',(-6.,61.831249998771,-3.46410161513776));
#8851=CARTESIAN_POINT('Ctrl Pts',(-6.,61.868749998771,-7.34788079488412E-16));
#8852=CARTESIAN_POINT('Ctrl Pts',(-6.,61.906249998771,3.46410161513775));
#8853=CARTESIAN_POINT('Ctrl Pts',(-3.,61.943749998771,5.19615242270663));
#8854=CARTESIAN_POINT('Ctrl Pts',(-1.27269028646989E-15,61.981249998771,
6.92820323027551));
#8855=CARTESIAN_POINT('Ctrl Pts',(3.,62.018749998771,5.19615242270663));
#8856=CARTESIAN_POINT('Ctrl Pts',(6.,62.056249998771,3.46410161513776));
#8857=CARTESIAN_POINT('Ctrl Pts',(6.,62.093749998771,0.));
#8858=CARTESIAN_POINT('Ctrl Pts',(6.,62.131249998771,-3.46410161513775));
#8859=CARTESIAN_POINT('Ctrl Pts',(3.,62.168749998771,-5.19615242270663));
#8860=CARTESIAN_POINT('Ctrl Pts',(4.24230095489963E-16,62.206249998771,
-6.92820323027551));
#8861=CARTESIAN_POINT('Ctrl Pts',(-3.,62.243749998771,-5.19615242270663));
#8862=CARTESIAN_POINT('Ctrl Pts',(-6.,62.281249998771,-3.46410161513776));
#8863=CARTESIAN_POINT('Ctrl Pts',(-6.,62.318749998771,-7.34788079488412E-16));
#8864=CARTESIAN_POINT('Ctrl Pts',(-6.,62.356249998771,3.46410161513775));
#8865=CARTESIAN_POINT('Ctrl Pts',(-3.,62.393749998771,5.19615242270663));
#8866=CARTESIAN_POINT('Ctrl Pts',(5.75643035625,50.2531249993855,0.));
#8867=CARTESIAN_POINT('Ctrl Pts',(5.75643035625,50.2906249993855,-3.32347661575227));
#8868=CARTESIAN_POINT('Ctrl Pts',(2.878215178125,50.3281249993855,-4.9852149236284));
#8869=CARTESIAN_POINT('Ctrl Pts',(4.0700849995221E-16,50.3656249993855,
-6.64695323150454));
#8870=CARTESIAN_POINT('Ctrl Pts',(-2.878215178125,50.4031249993855,-4.9852149236284));
#8871=CARTESIAN_POINT('Ctrl Pts',(-5.75643035625,50.4406249993855,-3.32347661575227));
#8872=CARTESIAN_POINT('Ctrl Pts',(-5.75643035625,50.4781249993855,-7.04959401029622E-16));
#8873=CARTESIAN_POINT('Ctrl Pts',(-5.75643035625,50.5156249993855,3.32347661575227));
#8874=CARTESIAN_POINT('Ctrl Pts',(-2.878215178125,50.5531249993855,4.9852149236284));
#8875=CARTESIAN_POINT('Ctrl Pts',(-1.22102549985663E-15,50.5906249993855,
6.64695323150454));
#8876=CARTESIAN_POINT('Ctrl Pts',(2.878215178125,50.6281249993855,4.98521492362841));
#8877=CARTESIAN_POINT('Ctrl Pts',(5.75643035625,50.6656249993855,3.32347661575227));
#8878=CARTESIAN_POINT('Ctrl Pts',(5.75643035625,50.7031249993855,0.));
#8879=CARTESIAN_POINT('Ctrl Pts',(5.75643035625,50.7406249993855,-3.32347661575227));
#8880=CARTESIAN_POINT('Ctrl Pts',(2.878215178125,50.7781249993855,-4.9852149236284));
#8881=CARTESIAN_POINT('Ctrl Pts',(4.0700849995221E-16,50.8156249993855,
-6.64695323150454));
#8882=CARTESIAN_POINT('Ctrl Pts',(-2.878215178125,50.8531249993855,-4.9852149236284));
#8883=CARTESIAN_POINT('Ctrl Pts',(-5.75643035625,50.8906249993855,-3.32347661575227));
#8884=CARTESIAN_POINT('Ctrl Pts',(-5.75643035625,50.9281249993855,-7.04959401029622E-16));
#8885=CARTESIAN_POINT('Ctrl Pts',(-5.75643035625,50.9656249993855,3.32347661575227));
#8886=CARTESIAN_POINT('Ctrl Pts',(-2.878215178125,51.0031249993855,4.9852149236284));
#8887=CARTESIAN_POINT('Ctrl Pts',(-1.22102549985663E-15,51.0406249993855,
6.64695323150454));
#8888=CARTESIAN_POINT('Ctrl Pts',(2.878215178125,51.0781249993855,4.98521492362841));
#8889=CARTESIAN_POINT('Ctrl Pts',(5.75643035625,51.1156249993855,3.32347661575227));
#8890=CARTESIAN_POINT('Ctrl Pts',(5.75643035625,51.1531249993855,0.));
#8891=CARTESIAN_POINT('Ctrl Pts',(5.75643035625,51.1906249993855,-3.32347661575227));
#8892=CARTESIAN_POINT('Ctrl Pts',(2.878215178125,51.2281249993855,-4.9852149236284));
#8893=CARTESIAN_POINT('Ctrl Pts',(4.0700849995221E-16,51.2656249993855,
-6.64695323150454));
#8894=CARTESIAN_POINT('Ctrl Pts',(-2.878215178125,51.3031249993855,-4.9852149236284));
#8895=CARTESIAN_POINT('Ctrl Pts',(-5.75643035625,51.3406249993855,-3.32347661575227));
#8896=CARTESIAN_POINT('Ctrl Pts',(-5.75643035625,51.3781249993855,-7.04959401029622E-16));
#8897=CARTESIAN_POINT('Ctrl Pts',(-5.75643035625,51.4156249993855,3.32347661575227));
#8898=CARTESIAN_POINT('Ctrl Pts',(-2.878215178125,51.4531249993855,4.9852149236284));
#8899=CARTESIAN_POINT('Ctrl Pts',(-1.22102549985663E-15,51.4906249993855,
6.64695323150454));
#8900=CARTESIAN_POINT('Ctrl Pts',(2.878215178125,51.5281249993855,4.98521492362841));
#8901=CARTESIAN_POINT('Ctrl Pts',(5.75643035625,51.5656249993855,3.32347661575227));
#8902=CARTESIAN_POINT('Ctrl Pts',(5.75643035625,51.6031249993855,0.));
#8903=CARTESIAN_POINT('Ctrl Pts',(5.75643035625,51.6406249993855,-3.32347661575227));
#8904=CARTESIAN_POINT('Ctrl Pts',(2.878215178125,51.6781249993855,-4.9852149236284));
#8905=CARTESIAN_POINT('Ctrl Pts',(4.0700849995221E-16,51.7156249993855,
-6.64695323150454));
#8906=CARTESIAN_POINT('Ctrl Pts',(-2.878215178125,51.7531249993855,-4.9852149236284));
#8907=CARTESIAN_POINT('Ctrl Pts',(-5.75643035625,51.7906249993855,-3.32347661575227));
#8908=CARTESIAN_POINT('Ctrl Pts',(-5.75643035625,51.8281249993855,-7.04959401029622E-16));
#8909=CARTESIAN_POINT('Ctrl Pts',(-5.75643035625,51.8656249993855,3.32347661575227));
#8910=CARTESIAN_POINT('Ctrl Pts',(-2.878215178125,51.9031249993855,4.9852149236284));
#8911=CARTESIAN_POINT('Ctrl Pts',(-1.22102549985663E-15,51.9406249993855,
6.64695323150454));
#8912=CARTESIAN_POINT('Ctrl Pts',(2.878215178125,51.9781249993855,4.98521492362841));
#8913=CARTESIAN_POINT('Ctrl Pts',(5.75643035625,52.0156249993855,3.32347661575227));
#8914=CARTESIAN_POINT('Ctrl Pts',(5.75643035625,52.0531249993855,0.));
#8915=CARTESIAN_POINT('Ctrl Pts',(5.75643035625,52.0906249993855,-3.32347661575227));
#8916=CARTESIAN_POINT('Ctrl Pts',(2.878215178125,52.1281249993855,-4.9852149236284));
#8917=CARTESIAN_POINT('Ctrl Pts',(4.0700849995221E-16,52.1656249993855,
-6.64695323150454));
#8918=CARTESIAN_POINT('Ctrl Pts',(-2.878215178125,52.2031249993855,-4.9852149236284));
#8919=CARTESIAN_POINT('Ctrl Pts',(-5.75643035625,52.2406249993855,-3.32347661575227));
#8920=CARTESIAN_POINT('Ctrl Pts',(-5.75643035625,52.2781249993855,-7.04959401029622E-16));
#8921=CARTESIAN_POINT('Ctrl Pts',(-5.75643035625,52.3156249993855,3.32347661575227));
#8922=CARTESIAN_POINT('Ctrl Pts',(-2.878215178125,52.3531249993855,4.9852149236284));
#8923=CARTESIAN_POINT('Ctrl Pts',(-1.22102549985663E-15,52.3906249993855,
6.64695323150454));
#8924=CARTESIAN_POINT('Ctrl Pts',(2.878215178125,52.4281249993855,4.98521492362841));
#8925=CARTESIAN_POINT('Ctrl Pts',(5.75643035625,52.4656249993855,3.32347661575227));
#8926=CARTESIAN_POINT('Ctrl Pts',(5.75643035625,52.5031249993855,0.));
#8927=CARTESIAN_POINT('Ctrl Pts',(5.75643035625,52.5406249993855,-3.32347661575227));
#8928=CARTESIAN_POINT('Ctrl Pts',(2.878215178125,52.5781249993855,-4.9852149236284));
#8929=CARTESIAN_POINT('Ctrl Pts',(4.0700849995221E-16,52.6156249993855,
-6.64695323150454));
#8930=CARTESIAN_POINT('Ctrl Pts',(-2.878215178125,52.6531249993855,-4.9852149236284));
#8931=CARTESIAN_POINT('Ctrl Pts',(-5.75643035625,52.6906249993855,-3.32347661575227));
#8932=CARTESIAN_POINT('Ctrl Pts',(-5.75643035625,52.7281249993855,-7.04959401029622E-16));
#8933=CARTESIAN_POINT('Ctrl Pts',(-5.75643035625,52.7656249993855,3.32347661575227));
#8934=CARTESIAN_POINT('Ctrl Pts',(-2.878215178125,52.8031249993855,4.9852149236284));
#8935=CARTESIAN_POINT('Ctrl Pts',(-1.22102549985663E-15,52.8406249993855,
6.64695323150454));
#8936=CARTESIAN_POINT('Ctrl Pts',(2.878215178125,52.8781249993855,4.98521492362841));
#8937=CARTESIAN_POINT('Ctrl Pts',(5.75643035625,52.9156249993855,3.32347661575227));
#8938=CARTESIAN_POINT('Ctrl Pts',(5.75643035625,52.9531249993855,0.));
#8939=CARTESIAN_POINT('Ctrl Pts',(5.75643035625,52.9906249993855,-3.32347661575227));
#8940=CARTESIAN_POINT('Ctrl Pts',(2.878215178125,53.0281249993855,-4.9852149236284));
#8941=CARTESIAN_POINT('Ctrl Pts',(4.0700849995221E-16,53.0656249993855,
-6.64695323150454));
#8942=CARTESIAN_POINT('Ctrl Pts',(-2.878215178125,53.1031249993855,-4.9852149236284));
#8943=CARTESIAN_POINT('Ctrl Pts',(-5.75643035625,53.1406249993855,-3.32347661575227));
#8944=CARTESIAN_POINT('Ctrl Pts',(-5.75643035625,53.1781249993855,-7.04959401029622E-16));
#8945=CARTESIAN_POINT('Ctrl Pts',(-5.75643035625,53.2156249993855,3.32347661575227));
#8946=CARTESIAN_POINT('Ctrl Pts',(-2.878215178125,53.2531249993855,4.9852149236284));
#8947=CARTESIAN_POINT('Ctrl Pts',(-1.22102549985663E-15,53.2906249993855,
6.64695323150454));
#8948=CARTESIAN_POINT('Ctrl Pts',(2.878215178125,53.3281249993855,4.98521492362841));
#8949=CARTESIAN_POINT('Ctrl Pts',(5.75643035625,53.3656249993855,3.32347661575227));
#8950=CARTESIAN_POINT('Ctrl Pts',(5.75643035625,53.4031249993855,0.));
#8951=CARTESIAN_POINT('Ctrl Pts',(5.75643035625,53.4406249993855,-3.32347661575227));
#8952=CARTESIAN_POINT('Ctrl Pts',(2.878215178125,53.4781249993855,-4.9852149236284));
#8953=CARTESIAN_POINT('Ctrl Pts',(4.0700849995221E-16,53.5156249993855,
-6.64695323150454));
#8954=CARTESIAN_POINT('Ctrl Pts',(-2.878215178125,53.5531249993855,-4.9852149236284));
#8955=CARTESIAN_POINT('Ctrl Pts',(-5.75643035625,53.5906249993855,-3.32347661575227));
#8956=CARTESIAN_POINT('Ctrl Pts',(-5.75643035625,53.6281249993855,-7.04959401029622E-16));
#8957=CARTESIAN_POINT('Ctrl Pts',(-5.75643035625,53.6656249993855,3.32347661575227));
#8958=CARTESIAN_POINT('Ctrl Pts',(-2.878215178125,53.7031249993855,4.9852149236284));
#8959=CARTESIAN_POINT('Ctrl Pts',(-1.22102549985663E-15,53.7406249993855,
6.64695323150454));
#8960=CARTESIAN_POINT('Ctrl Pts',(2.878215178125,53.7781249993855,4.98521492362841));
#8961=CARTESIAN_POINT('Ctrl Pts',(5.75643035625,53.8156249993855,3.32347661575227));
#8962=CARTESIAN_POINT('Ctrl Pts',(5.75643035625,53.8531249993855,0.));
#8963=CARTESIAN_POINT('Ctrl Pts',(5.75643035625,53.8906249993855,-3.32347661575227));
#8964=CARTESIAN_POINT('Ctrl Pts',(2.878215178125,53.9281249993855,-4.9852149236284));
#8965=CARTESIAN_POINT('Ctrl Pts',(4.0700849995221E-16,53.9656249993855,
-6.64695323150454));
#8966=CARTESIAN_POINT('Ctrl Pts',(-2.878215178125,54.0031249993855,-4.9852149236284));
#8967=CARTESIAN_POINT('Ctrl Pts',(-5.75643035625,54.0406249993855,-3.32347661575227));
#8968=CARTESIAN_POINT('Ctrl Pts',(-5.75643035625,54.0781249993855,-7.04959401029622E-16));
#8969=CARTESIAN_POINT('Ctrl Pts',(-5.75643035625,54.1156249993855,3.32347661575227));
#8970=CARTESIAN_POINT('Ctrl Pts',(-2.878215178125,54.1531249993855,4.9852149236284));
#8971=CARTESIAN_POINT('Ctrl Pts',(-1.22102549985663E-15,54.1906249993855,
6.64695323150454));
#8972=CARTESIAN_POINT('Ctrl Pts',(2.878215178125,54.2281249993855,4.98521492362841));
#8973=CARTESIAN_POINT('Ctrl Pts',(5.75643035625,54.2656249993855,3.32347661575227));
#8974=CARTESIAN_POINT('Ctrl Pts',(5.75643035625,54.3031249993855,0.));
#8975=CARTESIAN_POINT('Ctrl Pts',(5.75643035625,54.3406249993855,-3.32347661575227));
#8976=CARTESIAN_POINT('Ctrl Pts',(2.878215178125,54.3781249993855,-4.9852149236284));
#8977=CARTESIAN_POINT('Ctrl Pts',(4.0700849995221E-16,54.4156249993855,
-6.64695323150454));
#8978=CARTESIAN_POINT('Ctrl Pts',(-2.878215178125,54.4531249993855,-4.9852149236284));
#8979=CARTESIAN_POINT('Ctrl Pts',(-5.75643035625,54.4906249993855,-3.32347661575227));
#8980=CARTESIAN_POINT('Ctrl Pts',(-5.75643035625,54.5281249993855,-7.04959401029622E-16));
#8981=CARTESIAN_POINT('Ctrl Pts',(-5.75643035625,54.5656249993855,3.32347661575227));
#8982=CARTESIAN_POINT('Ctrl Pts',(-2.878215178125,54.6031249993855,4.9852149236284));
#8983=CARTESIAN_POINT('Ctrl Pts',(-1.22102549985663E-15,54.6406249993855,
6.64695323150454));
#8984=CARTESIAN_POINT('Ctrl Pts',(2.878215178125,54.6781249993855,4.98521492362841));
#8985=CARTESIAN_POINT('Ctrl Pts',(5.75643035625,54.7156249993855,3.32347661575227));
#8986=CARTESIAN_POINT('Ctrl Pts',(5.75643035625,54.7531249993855,0.));
#8987=CARTESIAN_POINT('Ctrl Pts',(5.75643035625,54.7906249993855,-3.32347661575227));
#8988=CARTESIAN_POINT('Ctrl Pts',(2.878215178125,54.8281249993855,-4.9852149236284));
#8989=CARTESIAN_POINT('Ctrl Pts',(4.0700849995221E-16,54.8656249993855,
-6.64695323150454));
#8990=CARTESIAN_POINT('Ctrl Pts',(-2.878215178125,54.9031249993855,-4.9852149236284));
#8991=CARTESIAN_POINT('Ctrl Pts',(-5.75643035625,54.9406249993855,-3.32347661575227));
#8992=CARTESIAN_POINT('Ctrl Pts',(-5.75643035625,54.9781249993855,-7.04959401029622E-16));
#8993=CARTESIAN_POINT('Ctrl Pts',(-5.75643035625,55.0156249993855,3.32347661575227));
#8994=CARTESIAN_POINT('Ctrl Pts',(-2.878215178125,55.0531249993855,4.9852149236284));
#8995=CARTESIAN_POINT('Ctrl Pts',(-1.22102549985663E-15,55.0906249993855,
6.64695323150454));
#8996=CARTESIAN_POINT('Ctrl Pts',(2.878215178125,55.1281249993855,4.98521492362841));
#8997=CARTESIAN_POINT('Ctrl Pts',(5.75643035625,55.1656249993855,3.32347661575227));
#8998=CARTESIAN_POINT('Ctrl Pts',(5.75643035625,55.2031249993855,0.));
#8999=CARTESIAN_POINT('Ctrl Pts',(5.75643035625,55.2406249993855,-3.32347661575227));
#9000=CARTESIAN_POINT('Ctrl Pts',(2.878215178125,55.2781249993855,-4.9852149236284));
#9001=CARTESIAN_POINT('Ctrl Pts',(4.0700849995221E-16,55.3156249993855,
-6.64695323150454));
#9002=CARTESIAN_POINT('Ctrl Pts',(-2.878215178125,55.3531249993855,-4.9852149236284));
#9003=CARTESIAN_POINT('Ctrl Pts',(-5.75643035625,55.3906249993855,-3.32347661575227));
#9004=CARTESIAN_POINT('Ctrl Pts',(-5.75643035625,55.4281249993855,-7.04959401029622E-16));
#9005=CARTESIAN_POINT('Ctrl Pts',(-5.75643035625,55.4656249993855,3.32347661575227));
#9006=CARTESIAN_POINT('Ctrl Pts',(-2.878215178125,55.5031249993855,4.9852149236284));
#9007=CARTESIAN_POINT('Ctrl Pts',(-1.22102549985663E-15,55.5406249993855,
6.64695323150454));
#9008=CARTESIAN_POINT('Ctrl Pts',(2.878215178125,55.5781249993855,4.98521492362841));
#9009=CARTESIAN_POINT('Ctrl Pts',(5.75643035625,55.6156249993855,3.32347661575227));
#9010=CARTESIAN_POINT('Ctrl Pts',(5.75643035625,55.6531249993855,0.));
#9011=CARTESIAN_POINT('Ctrl Pts',(5.75643035625,55.6906249993855,-3.32347661575227));
#9012=CARTESIAN_POINT('Ctrl Pts',(2.878215178125,55.7281249993855,-4.9852149236284));
#9013=CARTESIAN_POINT('Ctrl Pts',(4.0700849995221E-16,55.7656249993855,
-6.64695323150454));
#9014=CARTESIAN_POINT('Ctrl Pts',(-2.878215178125,55.8031249993855,-4.9852149236284));
#9015=CARTESIAN_POINT('Ctrl Pts',(-5.75643035625,55.8406249993855,-3.32347661575227));
#9016=CARTESIAN_POINT('Ctrl Pts',(-5.75643035625,55.8781249993855,-7.04959401029622E-16));
#9017=CARTESIAN_POINT('Ctrl Pts',(-5.75643035625,55.9156249993855,3.32347661575227));
#9018=CARTESIAN_POINT('Ctrl Pts',(-2.878215178125,55.9531249993855,4.9852149236284));
#9019=CARTESIAN_POINT('Ctrl Pts',(-1.22102549985663E-15,55.9906249993855,
6.64695323150454));
#9020=CARTESIAN_POINT('Ctrl Pts',(2.878215178125,56.0281249993855,4.98521492362841));
#9021=CARTESIAN_POINT('Ctrl Pts',(5.75643035625,56.0656249993855,3.32347661575227));
#9022=CARTESIAN_POINT('Ctrl Pts',(5.75643035625,56.1031249993855,0.));
#9023=CARTESIAN_POINT('Ctrl Pts',(5.75643035625,56.1406249993855,-3.32347661575227));
#9024=CARTESIAN_POINT('Ctrl Pts',(2.878215178125,56.1781249993855,-4.9852149236284));
#9025=CARTESIAN_POINT('Ctrl Pts',(4.0700849995221E-16,56.2156249993855,
-6.64695323150454));
#9026=CARTESIAN_POINT('Ctrl Pts',(-2.878215178125,56.2531249993855,-4.9852149236284));
#9027=CARTESIAN_POINT('Ctrl Pts',(-5.75643035625,56.2906249993855,-3.32347661575227));
#9028=CARTESIAN_POINT('Ctrl Pts',(-5.75643035625,56.3281249993855,-7.04959401029622E-16));
#9029=CARTESIAN_POINT('Ctrl Pts',(-5.75643035625,56.3656249993855,3.32347661575227));
#9030=CARTESIAN_POINT('Ctrl Pts',(-2.878215178125,56.4031249993855,4.9852149236284));
#9031=CARTESIAN_POINT('Ctrl Pts',(-1.22102549985663E-15,56.4406249993855,
6.64695323150454));
#9032=CARTESIAN_POINT('Ctrl Pts',(2.878215178125,56.4781249993855,4.98521492362841));
#9033=CARTESIAN_POINT('Ctrl Pts',(5.75643035625,56.5156249993855,3.32347661575227));
#9034=CARTESIAN_POINT('Ctrl Pts',(5.75643035625,56.5531249993855,0.));
#9035=CARTESIAN_POINT('Ctrl Pts',(5.75643035625,56.5906249993855,-3.32347661575227));
#9036=CARTESIAN_POINT('Ctrl Pts',(2.878215178125,56.6281249993855,-4.9852149236284));
#9037=CARTESIAN_POINT('Ctrl Pts',(4.0700849995221E-16,56.6656249993855,
-6.64695323150454));
#9038=CARTESIAN_POINT('Ctrl Pts',(-2.878215178125,56.7031249993855,-4.9852149236284));
#9039=CARTESIAN_POINT('Ctrl Pts',(-5.75643035625,56.7406249993855,-3.32347661575227));
#9040=CARTESIAN_POINT('Ctrl Pts',(-5.75643035625,56.7781249993855,-7.04959401029622E-16));
#9041=CARTESIAN_POINT('Ctrl Pts',(-5.75643035625,56.8156249993855,3.32347661575227));
#9042=CARTESIAN_POINT('Ctrl Pts',(-2.878215178125,56.8531249993855,4.9852149236284));
#9043=CARTESIAN_POINT('Ctrl Pts',(-1.22102549985663E-15,56.8906249993855,
6.64695323150454));
#9044=CARTESIAN_POINT('Ctrl Pts',(2.878215178125,56.9281249993855,4.98521492362841));
#9045=CARTESIAN_POINT('Ctrl Pts',(5.75643035625,56.9656249993855,3.32347661575227));
#9046=CARTESIAN_POINT('Ctrl Pts',(5.75643035625,57.0031249993855,0.));
#9047=CARTESIAN_POINT('Ctrl Pts',(5.75643035625,57.0406249993855,-3.32347661575227));
#9048=CARTESIAN_POINT('Ctrl Pts',(2.878215178125,57.0781249993855,-4.9852149236284));
#9049=CARTESIAN_POINT('Ctrl Pts',(4.0700849995221E-16,57.1156249993855,
-6.64695323150454));
#9050=CARTESIAN_POINT('Ctrl Pts',(-2.878215178125,57.1531249993855,-4.9852149236284));
#9051=CARTESIAN_POINT('Ctrl Pts',(-5.75643035625,57.1906249993855,-3.32347661575227));
#9052=CARTESIAN_POINT('Ctrl Pts',(-5.75643035625,57.2281249993855,-7.04959401029622E-16));
#9053=CARTESIAN_POINT('Ctrl Pts',(-5.75643035625,57.2656249993855,3.32347661575227));
#9054=CARTESIAN_POINT('Ctrl Pts',(-2.878215178125,57.3031249993855,4.9852149236284));
#9055=CARTESIAN_POINT('Ctrl Pts',(-1.22102549985663E-15,57.3406249993855,
6.64695323150454));
#9056=CARTESIAN_POINT('Ctrl Pts',(2.878215178125,57.3781249993855,4.98521492362841));
#9057=CARTESIAN_POINT('Ctrl Pts',(5.75643035625,57.4156249993855,3.32347661575227));
#9058=CARTESIAN_POINT('Ctrl Pts',(5.75643035625,57.4531249993855,0.));
#9059=CARTESIAN_POINT('Ctrl Pts',(5.75643035625,57.4906249993855,-3.32347661575227));
#9060=CARTESIAN_POINT('Ctrl Pts',(2.878215178125,57.5281249993855,-4.9852149236284));
#9061=CARTESIAN_POINT('Ctrl Pts',(4.0700849995221E-16,57.5656249993855,
-6.64695323150454));
#9062=CARTESIAN_POINT('Ctrl Pts',(-2.878215178125,57.6031249993855,-4.9852149236284));
#9063=CARTESIAN_POINT('Ctrl Pts',(-5.75643035625,57.6406249993855,-3.32347661575227));
#9064=CARTESIAN_POINT('Ctrl Pts',(-5.75643035625,57.6781249993855,-7.04959401029622E-16));
#9065=CARTESIAN_POINT('Ctrl Pts',(-5.75643035625,57.7156249993855,3.32347661575227));
#9066=CARTESIAN_POINT('Ctrl Pts',(-2.878215178125,57.7531249993855,4.9852149236284));
#9067=CARTESIAN_POINT('Ctrl Pts',(-1.22102549985663E-15,57.7906249993855,
6.64695323150454));
#9068=CARTESIAN_POINT('Ctrl Pts',(2.878215178125,57.8281249993855,4.98521492362841));
#9069=CARTESIAN_POINT('Ctrl Pts',(5.75643035625,57.8656249993855,3.32347661575227));
#9070=CARTESIAN_POINT('Ctrl Pts',(5.75643035625,57.9031249993855,0.));
#9071=CARTESIAN_POINT('Ctrl Pts',(5.75643035625,57.9406249993855,-3.32347661575227));
#9072=CARTESIAN_POINT('Ctrl Pts',(2.878215178125,57.9781249993855,-4.9852149236284));
#9073=CARTESIAN_POINT('Ctrl Pts',(4.0700849995221E-16,58.0156249993855,
-6.64695323150454));
#9074=CARTESIAN_POINT('Ctrl Pts',(-2.878215178125,58.0531249993855,-4.9852149236284));
#9075=CARTESIAN_POINT('Ctrl Pts',(-5.75643035625,58.0906249993855,-3.32347661575227));
#9076=CARTESIAN_POINT('Ctrl Pts',(-5.75643035625,58.1281249993855,-7.04959401029622E-16));
#9077=CARTESIAN_POINT('Ctrl Pts',(-5.75643035625,58.1656249993855,3.32347661575227));
#9078=CARTESIAN_POINT('Ctrl Pts',(-2.878215178125,58.2031249993855,4.9852149236284));
#9079=CARTESIAN_POINT('Ctrl Pts',(-1.22102549985663E-15,58.2406249993855,
6.64695323150454));
#9080=CARTESIAN_POINT('Ctrl Pts',(2.878215178125,58.2781249993855,4.98521492362841));
#9081=CARTESIAN_POINT('Ctrl Pts',(5.75643035625,58.3156249993855,3.32347661575227));
#9082=CARTESIAN_POINT('Ctrl Pts',(5.75643035625,58.3531249993855,0.));
#9083=CARTESIAN_POINT('Ctrl Pts',(5.75643035625,58.3906249993855,-3.32347661575227));
#9084=CARTESIAN_POINT('Ctrl Pts',(2.878215178125,58.4281249993855,-4.9852149236284));
#9085=CARTESIAN_POINT('Ctrl Pts',(4.0700849995221E-16,58.4656249993855,
-6.64695323150454));
#9086=CARTESIAN_POINT('Ctrl Pts',(-2.878215178125,58.5031249993855,-4.9852149236284));
#9087=CARTESIAN_POINT('Ctrl Pts',(-5.75643035625,58.5406249993855,-3.32347661575227));
#9088=CARTESIAN_POINT('Ctrl Pts',(-5.75643035625,58.5781249993855,-7.04959401029622E-16));
#9089=CARTESIAN_POINT('Ctrl Pts',(-5.75643035625,58.6156249993855,3.32347661575227));
#9090=CARTESIAN_POINT('Ctrl Pts',(-2.878215178125,58.6531249993855,4.9852149236284));
#9091=CARTESIAN_POINT('Ctrl Pts',(-1.22102549985663E-15,58.6906249993855,
6.64695323150454));
#9092=CARTESIAN_POINT('Ctrl Pts',(2.878215178125,58.7281249993855,4.98521492362841));
#9093=CARTESIAN_POINT('Ctrl Pts',(5.75643035625,58.7656249993855,3.32347661575227));
#9094=CARTESIAN_POINT('Ctrl Pts',(5.75643035625,58.8031249993855,0.));
#9095=CARTESIAN_POINT('Ctrl Pts',(5.75643035625,58.8406249993855,-3.32347661575227));
#9096=CARTESIAN_POINT('Ctrl Pts',(2.878215178125,58.8781249993855,-4.9852149236284));
#9097=CARTESIAN_POINT('Ctrl Pts',(4.0700849995221E-16,58.9156249993855,
-6.64695323150454));
#9098=CARTESIAN_POINT('Ctrl Pts',(-2.878215178125,58.9531249993855,-4.9852149236284));
#9099=CARTESIAN_POINT('Ctrl Pts',(-5.75643035625,58.9906249993855,-3.32347661575227));
#9100=CARTESIAN_POINT('Ctrl Pts',(-5.75643035625,59.0281249993855,-7.04959401029622E-16));
#9101=CARTESIAN_POINT('Ctrl Pts',(-5.75643035625,59.0656249993855,3.32347661575227));
#9102=CARTESIAN_POINT('Ctrl Pts',(-2.878215178125,59.1031249993855,4.9852149236284));
#9103=CARTESIAN_POINT('Ctrl Pts',(-1.22102549985663E-15,59.1406249993855,
6.64695323150454));
#9104=CARTESIAN_POINT('Ctrl Pts',(2.878215178125,59.1781249993855,4.98521492362841));
#9105=CARTESIAN_POINT('Ctrl Pts',(5.75643035625,59.2156249993855,3.32347661575227));
#9106=CARTESIAN_POINT('Ctrl Pts',(5.75643035625,59.2531249993855,0.));
#9107=CARTESIAN_POINT('Ctrl Pts',(5.75643035625,59.2906249993855,-3.32347661575227));
#9108=CARTESIAN_POINT('Ctrl Pts',(2.878215178125,59.3281249993855,-4.9852149236284));
#9109=CARTESIAN_POINT('Ctrl Pts',(4.0700849995221E-16,59.3656249993855,
-6.64695323150454));
#9110=CARTESIAN_POINT('Ctrl Pts',(-2.878215178125,59.4031249993855,-4.9852149236284));
#9111=CARTESIAN_POINT('Ctrl Pts',(-5.75643035625,59.4406249993855,-3.32347661575227));
#9112=CARTESIAN_POINT('Ctrl Pts',(-5.75643035625,59.4781249993855,-7.04959401029622E-16));
#9113=CARTESIAN_POINT('Ctrl Pts',(-5.75643035625,59.5156249993855,3.32347661575227));
#9114=CARTESIAN_POINT('Ctrl Pts',(-2.878215178125,59.5531249993855,4.9852149236284));
#9115=CARTESIAN_POINT('Ctrl Pts',(-1.22102549985663E-15,59.5906249993855,
6.64695323150454));
#9116=CARTESIAN_POINT('Ctrl Pts',(2.878215178125,59.6281249993855,4.98521492362841));
#9117=CARTESIAN_POINT('Ctrl Pts',(5.75643035625,59.6656249993855,3.32347661575227));
#9118=CARTESIAN_POINT('Ctrl Pts',(5.75643035625,59.7031249993855,0.));
#9119=CARTESIAN_POINT('Ctrl Pts',(5.75643035625,59.7406249993855,-3.32347661575227));
#9120=CARTESIAN_POINT('Ctrl Pts',(2.878215178125,59.7781249993855,-4.9852149236284));
#9121=CARTESIAN_POINT('Ctrl Pts',(4.0700849995221E-16,59.8156249993855,
-6.64695323150454));
#9122=CARTESIAN_POINT('Ctrl Pts',(-2.878215178125,59.8531249993855,-4.9852149236284));
#9123=CARTESIAN_POINT('Ctrl Pts',(-5.75643035625,59.8906249993855,-3.32347661575227));
#9124=CARTESIAN_POINT('Ctrl Pts',(-5.75643035625,59.9281249993855,-7.04959401029622E-16));
#9125=CARTESIAN_POINT('Ctrl Pts',(-5.75643035625,59.9656249993855,3.32347661575227));
#9126=CARTESIAN_POINT('Ctrl Pts',(-2.878215178125,60.0031249993855,4.9852149236284));
#9127=CARTESIAN_POINT('Ctrl Pts',(-1.22102549985663E-15,60.0406249993855,
6.64695323150454));
#9128=CARTESIAN_POINT('Ctrl Pts',(2.878215178125,60.0781249993855,4.98521492362841));
#9129=CARTESIAN_POINT('Ctrl Pts',(5.75643035625,60.1156249993855,3.32347661575227));
#9130=CARTESIAN_POINT('Ctrl Pts',(5.75643035625,60.1531249993855,0.));
#9131=CARTESIAN_POINT('Ctrl Pts',(5.75643035625,60.1906249993855,-3.32347661575227));
#9132=CARTESIAN_POINT('Ctrl Pts',(2.878215178125,60.2281249993855,-4.9852149236284));
#9133=CARTESIAN_POINT('Ctrl Pts',(4.0700849995221E-16,60.2656249993855,
-6.64695323150454));
#9134=CARTESIAN_POINT('Ctrl Pts',(-2.878215178125,60.3031249993855,-4.9852149236284));
#9135=CARTESIAN_POINT('Ctrl Pts',(-5.75643035625,60.3406249993855,-3.32347661575227));
#9136=CARTESIAN_POINT('Ctrl Pts',(-5.75643035625,60.3781249993855,-7.04959401029622E-16));
#9137=CARTESIAN_POINT('Ctrl Pts',(-5.75643035625,60.4156249993855,3.32347661575227));
#9138=CARTESIAN_POINT('Ctrl Pts',(-2.878215178125,60.4531249993855,4.9852149236284));
#9139=CARTESIAN_POINT('Ctrl Pts',(-1.22102549985663E-15,60.4906249993855,
6.64695323150454));
#9140=CARTESIAN_POINT('Ctrl Pts',(2.878215178125,60.5281249993855,4.98521492362841));
#9141=CARTESIAN_POINT('Ctrl Pts',(5.75643035625,60.5656249993855,3.32347661575227));
#9142=CARTESIAN_POINT('Ctrl Pts',(5.75643035625,60.6031249993855,0.));
#9143=CARTESIAN_POINT('Ctrl Pts',(5.75643035625,60.6406249993855,-3.32347661575227));
#9144=CARTESIAN_POINT('Ctrl Pts',(2.878215178125,60.6781249993855,-4.9852149236284));
#9145=CARTESIAN_POINT('Ctrl Pts',(4.0700849995221E-16,60.7156249993855,
-6.64695323150454));
#9146=CARTESIAN_POINT('Ctrl Pts',(-2.878215178125,60.7531249993855,-4.9852149236284));
#9147=CARTESIAN_POINT('Ctrl Pts',(-5.75643035625,60.7906249993855,-3.32347661575227));
#9148=CARTESIAN_POINT('Ctrl Pts',(-5.75643035625,60.8281249993855,-7.04959401029622E-16));
#9149=CARTESIAN_POINT('Ctrl Pts',(-5.75643035625,60.8656249993855,3.32347661575227));
#9150=CARTESIAN_POINT('Ctrl Pts',(-2.878215178125,60.9031249993855,4.9852149236284));
#9151=CARTESIAN_POINT('Ctrl Pts',(-1.22102549985663E-15,60.9406249993855,
6.64695323150454));
#9152=CARTESIAN_POINT('Ctrl Pts',(2.878215178125,60.9781249993855,4.98521492362841));
#9153=CARTESIAN_POINT('Ctrl Pts',(5.75643035625,61.0156249993855,3.32347661575227));
#9154=CARTESIAN_POINT('Ctrl Pts',(5.75643035625,61.0531249993855,0.));
#9155=CARTESIAN_POINT('Ctrl Pts',(5.75643035625,61.0906249993855,-3.32347661575227));
#9156=CARTESIAN_POINT('Ctrl Pts',(2.878215178125,61.1281249993855,-4.9852149236284));
#9157=CARTESIAN_POINT('Ctrl Pts',(4.0700849995221E-16,61.1656249993855,
-6.64695323150454));
#9158=CARTESIAN_POINT('Ctrl Pts',(-2.878215178125,61.2031249993855,-4.9852149236284));
#9159=CARTESIAN_POINT('Ctrl Pts',(-5.75643035625,61.2406249993855,-3.32347661575227));
#9160=CARTESIAN_POINT('Ctrl Pts',(-5.75643035625,61.2781249993855,-7.04959401029622E-16));
#9161=CARTESIAN_POINT('Ctrl Pts',(-5.75643035625,61.3156249993855,3.32347661575227));
#9162=CARTESIAN_POINT('Ctrl Pts',(-2.878215178125,61.3531249993855,4.9852149236284));
#9163=CARTESIAN_POINT('Ctrl Pts',(-1.22102549985663E-15,61.3906249993855,
6.64695323150454));
#9164=CARTESIAN_POINT('Ctrl Pts',(2.878215178125,61.4281249993855,4.98521492362841));
#9165=CARTESIAN_POINT('Ctrl Pts',(5.75643035625,61.4656249993855,3.32347661575227));
#9166=CARTESIAN_POINT('Ctrl Pts',(5.75643035625,61.5031249993855,0.));
#9167=CARTESIAN_POINT('Ctrl Pts',(5.75643035625,61.5406249993855,-3.32347661575227));
#9168=CARTESIAN_POINT('Ctrl Pts',(2.878215178125,61.5781249993855,-4.9852149236284));
#9169=CARTESIAN_POINT('Ctrl Pts',(4.0700849995221E-16,61.6156249993855,
-6.64695323150454));
#9170=CARTESIAN_POINT('Ctrl Pts',(-2.878215178125,61.6531249993855,-4.9852149236284));
#9171=CARTESIAN_POINT('Ctrl Pts',(-5.75643035625,61.6906249993855,-3.32347661575227));
#9172=CARTESIAN_POINT('Ctrl Pts',(-5.75643035625,61.7281249993855,-7.04959401029622E-16));
#9173=CARTESIAN_POINT('Ctrl Pts',(-5.75643035625,61.7656249993855,3.32347661575227));
#9174=CARTESIAN_POINT('Ctrl Pts',(-2.878215178125,61.8031249993855,4.9852149236284));
#9175=CARTESIAN_POINT('Ctrl Pts',(-1.22102549985663E-15,61.8406249993855,
6.64695323150454));
#9176=CARTESIAN_POINT('Ctrl Pts',(2.878215178125,61.8781249993855,4.98521492362841));
#9177=CARTESIAN_POINT('Ctrl Pts',(5.75643035625,61.9156249993855,3.32347661575227));
#9178=CARTESIAN_POINT('Ctrl Pts',(5.75643035625,61.9531249993855,0.));
#9179=CARTESIAN_POINT('Ctrl Pts',(5.75643035625,61.9906249993855,-3.32347661575227));
#9180=CARTESIAN_POINT('Ctrl Pts',(2.878215178125,62.0281249993855,-4.9852149236284));
#9181=CARTESIAN_POINT('Ctrl Pts',(4.0700849995221E-16,62.0656249993855,
-6.64695323150454));
#9182=CARTESIAN_POINT('Ctrl Pts',(-2.878215178125,62.1031249993855,-4.9852149236284));
#9183=CARTESIAN_POINT('Ctrl Pts',(-5.75643035625,62.1406249993855,-3.32347661575227));
#9184=CARTESIAN_POINT('Ctrl Pts',(-5.75643035625,62.1781249993855,-7.04959401029622E-16));
#9185=CARTESIAN_POINT('Ctrl Pts',(-5.75643035625,62.2156249993855,3.32347661575227));
#9186=CARTESIAN_POINT('Ctrl Pts',(-2.878215178125,62.2531249993855,4.9852149236284));
#9187=CARTESIAN_POINT('',(0.,0.,0.));
#9188=CARTESIAN_POINT('Origin',(0.,63.,0.));
#9189=CARTESIAN_POINT('',(-1.83697019872103E-15,63.,15.));
#9190=CARTESIAN_POINT('Origin',(0.,63.,0.));
#9191=CARTESIAN_POINT('',(-1.83697019872103E-15,55.,15.));
#9192=CARTESIAN_POINT('',(-1.83697019872103E-15,63.,15.));
#9193=CARTESIAN_POINT('Origin',(0.,55.,0.));
#9194=CARTESIAN_POINT('Origin',(0.,67.,0.));
#9195=CARTESIAN_POINT('',(3.67394039744206E-15,67.,-30.));
#9196=CARTESIAN_POINT('',(-3.67394039744206E-15,67.,30.));
#9197=CARTESIAN_POINT('Origin',(0.,67.,0.));
#9198=CARTESIAN_POINT('Origin',(0.,67.,0.));
#9199=CARTESIAN_POINT('',(-2.93915231795365E-15,73.,24.));
#9200=CARTESIAN_POINT('',(-3.67394039744206E-15,67.,30.));
#9201=CARTESIAN_POINT('Origin',(0.,73.,0.));
#9202=CARTESIAN_POINT('Origin',(0.,55.,0.));
#9203=CARTESIAN_POINT('',(-3.67394039744206E-15,55.,-30.));
#9204=CARTESIAN_POINT('',(-3.67394039744206E-15,55.,-30.));
#9205=CARTESIAN_POINT('Origin',(0.,55.,0.));
#9206=CARTESIAN_POINT('Origin',(0.,55.,0.));
#9207=CARTESIAN_POINT('',(-7.34788079488412E-16,63.,-6.));
#9208=CARTESIAN_POINT('Origin',(0.,63.,0.));
#9209=CARTESIAN_POINT('',(-7.34788079488412E-16,73.,-6.));
#9210=CARTESIAN_POINT('',(-7.34788079488412E-16,55.,-6.));
#9211=CARTESIAN_POINT('Origin',(0.,73.,0.));
#9212=CARTESIAN_POINT('Origin',(0.,55.,0.));
#9213=CARTESIAN_POINT('Origin',(0.,73.,0.));
#9214=CARTESIAN_POINT('Origin',(0.,63.,0.));
#9215=CARTESIAN_POINT('',(0.,0.,0.));
#9216=CARTESIAN_POINT('Origin',(18.1535684584702,322.954137916175,6.2));
#9217=CARTESIAN_POINT('',(16.1535684584702,322.954137916175,-4.));
#9218=CARTESIAN_POINT('Origin',(18.1535684584702,322.954137916175,-4.));
#9219=CARTESIAN_POINT('',(16.1535684584702,322.954137916175,4.));
#9220=CARTESIAN_POINT('',(16.1535684584702,322.954137916175,6.2));
#9221=CARTESIAN_POINT('Origin',(18.1535684584702,322.954137916175,4.));
#9222=CARTESIAN_POINT('Origin',(0.,323.,0.));
#9223=CARTESIAN_POINT('',(6.25,323.,0.));
#9224=CARTESIAN_POINT('',(-7.65404249467096E-16,323.,6.25));
#9225=CARTESIAN_POINT('Origin',(0.,323.,0.));
#9226=CARTESIAN_POINT('',(-7.65404249467096E-16,320.,6.25));
#9227=CARTESIAN_POINT('',(-7.65404249467096E-16,323.,6.25));
#9228=CARTESIAN_POINT('Origin',(0.,320.,0.));
#9229=CARTESIAN_POINT('Origin',(0.,323.,0.));
#9230=CARTESIAN_POINT('Origin',(0.,323.,0.));
#9231=CARTESIAN_POINT('',(10.5148704224065,323.,-4.));
#9232=CARTESIAN_POINT('',(10.5148704224065,323.,4.));
#9233=CARTESIAN_POINT('Origin',(0.,323.,0.));
#9234=CARTESIAN_POINT('',(10.5148704224065,320.,-4.));
#9235=CARTESIAN_POINT('',(10.5148704224065,323.,-4.));
#9236=CARTESIAN_POINT('',(10.5148704224065,320.,4.));
#9237=CARTESIAN_POINT('Origin',(0.,320.,0.));
#9238=CARTESIAN_POINT('',(10.5148704224065,323.,4.));
#9239=CARTESIAN_POINT('Origin',(0.,323.,0.));
#9240=CARTESIAN_POINT('',(6.25,323.,4.));
#9241=CARTESIAN_POINT('',(0.,323.,4.));
#9242=CARTESIAN_POINT('',(6.25,323.,0.));
#9243=CARTESIAN_POINT('',(6.25,323.,-4.));
#9244=CARTESIAN_POINT('',(6.25,323.,0.));
#9245=CARTESIAN_POINT('',(0.,323.,-4.));
#9246=CARTESIAN_POINT('Origin',(0.,320.,0.));
#9247=CARTESIAN_POINT('',(18.25,320.,-4.));
#9248=CARTESIAN_POINT('',(6.25,320.,-4.));
#9249=CARTESIAN_POINT('',(18.25,320.,4.));
#9250=CARTESIAN_POINT('',(18.25,320.,4.));
#9251=CARTESIAN_POINT('',(6.25,320.,4.));
#9252=CARTESIAN_POINT('Origin',(6.25,326.,4.));
#9253=CARTESIAN_POINT('',(18.25,326.,4.));
#9254=CARTESIAN_POINT('Origin',(18.25,323.,4.));
#9255=CARTESIAN_POINT('',(10.8325756949558,326.,4.));
#9256=CARTESIAN_POINT('',(6.25,326.,4.));
#9257=CARTESIAN_POINT('Origin',(10.8325756949558,321.,4.));
#9258=CARTESIAN_POINT('Origin',(6.25,326.,-4.));
#9259=CARTESIAN_POINT('',(18.25,326.,-4.));
#9260=CARTESIAN_POINT('Origin',(18.25,323.,-4.));
#9261=CARTESIAN_POINT('',(10.8325756949558,326.,-4.));
#9262=CARTESIAN_POINT('Origin',(10.8325756949558,321.,-4.));
#9263=CARTESIAN_POINT('',(6.25,326.,-4.));
#9264=CARTESIAN_POINT('Origin',(0.,326.,0.));
#9265=CARTESIAN_POINT('',(18.25,326.,-4.));
#9266=CARTESIAN_POINT('',(10.8325756949558,326.,0.));
#9267=CARTESIAN_POINT('Origin',(10.8325756949558,321.,4.));
#9268=CARTESIAN_POINT('Origin',(18.25,323.,-4.));
#9269=CARTESIAN_POINT('',(0.,0.,0.));
#9270=CARTESIAN_POINT('Origin',(32.,329.539392014169,6.2));
#9271=CARTESIAN_POINT('',(30.,329.539392014169,4.2));
#9272=CARTESIAN_POINT('Origin',(32.,329.539392014169,4.2));
#9273=CARTESIAN_POINT('',(30.,329.539392014169,6.2));
#9274=CARTESIAN_POINT('',(30.,329.539392014169,6.2));
#9275=CARTESIAN_POINT('Origin',(32.,329.539392014169,6.2));
#9276=CARTESIAN_POINT('Origin',(32.,329.539392014169,6.2));
#9277=CARTESIAN_POINT('',(30.,329.539392014169,-6.2));
#9278=CARTESIAN_POINT('Origin',(32.,329.539392014169,-6.2));
#9279=CARTESIAN_POINT('',(30.,329.539392014169,-4.2));
#9280=CARTESIAN_POINT('',(30.,329.539392014169,6.2));
#9281=CARTESIAN_POINT('Origin',(32.,329.539392014169,-4.2));
#9282=CARTESIAN_POINT('Origin',(18.1535684584702,322.954137916175,6.2));
#9283=CARTESIAN_POINT('',(16.1535684584702,322.954137916175,4.2));
#9284=CARTESIAN_POINT('Origin',(18.1535684584702,322.954137916175,4.2));
#9285=CARTESIAN_POINT('',(16.1535684584702,322.954137916175,6.2));
#9286=CARTESIAN_POINT('',(16.1535684584702,322.954137916175,6.2));
#9287=CARTESIAN_POINT('Origin',(18.1535684584702,322.954137916175,6.2));
#9288=CARTESIAN_POINT('Origin',(18.1535684584702,322.954137916175,6.2));
#9289=CARTESIAN_POINT('',(16.1535684584702,322.954137916175,-6.2));
#9290=CARTESIAN_POINT('Origin',(18.1535684584702,322.954137916175,-6.2));
#9291=CARTESIAN_POINT('',(16.1535684584702,322.954137916175,-4.2));
#9292=CARTESIAN_POINT('',(16.1535684584702,322.954137916175,6.2));
#9293=CARTESIAN_POINT('Origin',(18.1535684584702,322.954137916175,-4.2));
#9294=CARTESIAN_POINT('Origin',(18.1535684584702,322.954137916175,6.2));
#9295=CARTESIAN_POINT('',(16.4355961689821,326.566418527167,6.2));
#9296=CARTESIAN_POINT('',(19.8715407479584,319.341857305183,6.2));
#9297=CARTESIAN_POINT('Origin',(18.1535684584702,322.954137916175,6.2));
#9298=CARTESIAN_POINT('',(16.4355961689821,326.566418527167,4.2));
#9299=CARTESIAN_POINT('',(16.4355961689821,326.566418527167,6.2));
#9300=CARTESIAN_POINT('',(19.8715407479584,319.341857305183,4.2));
#9301=CARTESIAN_POINT('Origin',(18.1535684584702,322.954137916175,4.2));
#9302=CARTESIAN_POINT('',(19.8715407479584,319.341857305183,4.2));
#9303=CARTESIAN_POINT('Origin',(30.3371238124307,325.901419668918,6.2));
#9304=CARTESIAN_POINT('',(32.0335381771776,325.126007768091,4.2));
#9305=CARTESIAN_POINT('',(57.6219164018174,313.429848262148,4.2));
#9306=CARTESIAN_POINT('',(30.3371238124307,325.901419668918,4.2));
#9307=CARTESIAN_POINT('',(57.6219164018174,313.429848262148,-4.20000000000002));
#9308=CARTESIAN_POINT('',(57.6219164018174,313.429848262148,-80.4294540302737));
#9309=CARTESIAN_POINT('',(32.0335381771776,325.126007768091,-4.2));
#9310=CARTESIAN_POINT('',(30.3371238124307,325.901419668918,-4.2));
#9311=CARTESIAN_POINT('',(32.0335381771776,325.126007768091,-6.2));
#9312=CARTESIAN_POINT('',(32.0335381771776,325.126007768091,-6.2));
#9313=CARTESIAN_POINT('',(121.28643244372,284.329514979686,-6.2));
#9314=CARTESIAN_POINT('',(30.3371238124307,325.901419668918,-6.2));
#9315=CARTESIAN_POINT('',(121.28643244372,284.329514979686,6.2));
#9316=CARTESIAN_POINT('',(121.28643244372,284.329514979686,6.2));
#9317=CARTESIAN_POINT('',(32.0335381771776,325.126007768091,6.2));
#9318=CARTESIAN_POINT('',(30.3371238124307,325.901419668918,6.2));
#9319=CARTESIAN_POINT('',(32.0335381771776,325.126007768091,6.2));
#9320=CARTESIAN_POINT('Origin',(124.612184818858,291.605459670189,6.2));
#9321=CARTESIAN_POINT('',(124.612184818858,291.605459670189,-6.2));
#9322=CARTESIAN_POINT('',(124.612184818858,291.605459670189,-6.2));
#9323=CARTESIAN_POINT('',(124.612184818858,291.605459670189,6.2));
#9324=CARTESIAN_POINT('',(124.612184818858,291.605459670189,6.2));
#9325=CARTESIAN_POINT('',(124.612184818858,291.605459670189,6.2));
#9326=CARTESIAN_POINT('Origin',(33.6628761875693,333.177364359421,6.2));
#9327=CARTESIAN_POINT('',(31.9664618228224,333.952776260248,6.2));
#9328=CARTESIAN_POINT('',(33.6628761875693,333.177364359421,6.2));
#9329=CARTESIAN_POINT('',(31.9664618228224,333.952776260248,-6.2));
#9330=CARTESIAN_POINT('',(33.6628761875693,333.177364359421,-6.2));
#9331=CARTESIAN_POINT('',(31.9664618228224,333.952776260248,-4.2));
#9332=CARTESIAN_POINT('',(31.9664618228224,333.952776260248,-6.2));
#9333=CARTESIAN_POINT('',(60.9476687769559,320.705792952651,-4.2));
#9334=CARTESIAN_POINT('',(33.6628761875693,333.177364359421,-4.2));
#9335=CARTESIAN_POINT('',(60.9476687769559,320.705792952651,4.19999999999997));
#9336=CARTESIAN_POINT('',(60.9476687769559,320.705792952651,-80.4294540302737));
#9337=CARTESIAN_POINT('',(31.9664618228224,333.952776260248,4.2));
#9338=CARTESIAN_POINT('',(33.6628761875693,333.177364359421,4.2));
#9339=CARTESIAN_POINT('',(31.9664618228224,333.952776260248,6.2));
#9340=CARTESIAN_POINT('Origin',(12.8233155579898,324.848446237679,6.2));
#9341=CARTESIAN_POINT('',(12.8233155579898,324.848446237679,4.2));
#9342=CARTESIAN_POINT('',(12.8233155579898,324.848446237679,6.2));
#9343=CARTESIAN_POINT('Origin',(16.2592601369661,317.623885015694,6.2));
#9344=CARTESIAN_POINT('',(16.2592601369661,317.623885015694,6.2));
#9345=CARTESIAN_POINT('',(16.2592601369661,317.623885015694,4.2));
#9346=CARTESIAN_POINT('Origin',(0.,0.,6.2));
#9347=CARTESIAN_POINT('Origin',(0.,0.,4.2));
#9348=CARTESIAN_POINT('',(-70.8422565789511,32.3811976450479,4.2));
#9349=CARTESIAN_POINT('Origin',(57.6219164018174,313.429848262148,-80.4294540302737));
#9350=CARTESIAN_POINT('',(57.6219164018174,313.429848262148,-4.2));
#9351=CARTESIAN_POINT('Origin',(12.8233155579898,324.848446237679,-6.2));
#9352=CARTESIAN_POINT('',(16.4355961689821,326.566418527167,-4.2));
#9353=CARTESIAN_POINT('',(12.8233155579898,324.848446237679,-4.2));
#9354=CARTESIAN_POINT('',(16.4355961689821,326.566418527167,-6.2));
#9355=CARTESIAN_POINT('',(12.8233155579898,324.848446237679,-6.2));
#9356=CARTESIAN_POINT('',(16.4355961689821,326.566418527167,-6.2));
#9357=CARTESIAN_POINT('Origin',(16.2592601369661,317.623885015694,-6.2));
#9358=CARTESIAN_POINT('',(19.8715407479584,319.341857305183,-6.2));
#9359=CARTESIAN_POINT('',(16.2592601369661,317.623885015694,-6.2));
#9360=CARTESIAN_POINT('',(19.8715407479584,319.341857305183,-4.2));
#9361=CARTESIAN_POINT('',(16.2592601369661,317.623885015694,-4.2));
#9362=CARTESIAN_POINT('',(19.8715407479584,319.341857305183,-4.2));
#9363=CARTESIAN_POINT('Origin',(0.,0.,-6.2));
#9364=CARTESIAN_POINT('Origin',(18.1535684584702,322.954137916175,-6.2));
#9365=CARTESIAN_POINT('Origin',(0.,0.,-4.2));
#9366=CARTESIAN_POINT('Origin',(18.1535684584702,322.954137916175,-4.2));
#9367=CARTESIAN_POINT('Origin',(18.1535684584702,322.954137916175,-6.2));
#9368=CARTESIAN_POINT('',(0.,0.,0.));
#9369=CARTESIAN_POINT('Ctrl Pts',(-8.,285.498925943689,0.0327551936971979));
#9370=CARTESIAN_POINT('Ctrl Pts',(-8.00877672769909,285.636425943689,-2.11083834575178));
#9371=CARTESIAN_POINT('Ctrl Pts',(-6.94458082712411,285.773925943689,-3.97163317015235));
#9372=CARTESIAN_POINT('Ctrl Pts',(-5.88038492654913,285.911425943689,-5.83242799455291));
#9373=CARTESIAN_POINT('Ctrl Pts',(-4.02836682984766,286.048925943689,-6.91182563342691));
#9374=CARTESIAN_POINT('Ctrl Pts',(-2.17634873314618,286.186425943689,-7.99122327230091));
#9375=CARTESIAN_POINT('Ctrl Pts',(-0.0327551936971984,286.323925943689,
-8.));
#9376=CARTESIAN_POINT('Ctrl Pts',(2.11083834575178,286.461425943689,-8.00877672769909));
#9377=CARTESIAN_POINT('Ctrl Pts',(3.97163317015235,286.598925943689,-6.94458082712411));
#9378=CARTESIAN_POINT('Ctrl Pts',(5.83242799455291,286.736425943689,-5.88038492654913));
#9379=CARTESIAN_POINT('Ctrl Pts',(6.91182563342691,286.873925943689,-4.02836682984766));
#9380=CARTESIAN_POINT('Ctrl Pts',(7.99122327230091,287.011425943689,-2.17634873314618));
#9381=CARTESIAN_POINT('Ctrl Pts',(8.,287.148925943689,-0.0327551936971989));
#9382=CARTESIAN_POINT('Ctrl Pts',(8.00877672769909,287.286425943689,2.11083834575178));
#9383=CARTESIAN_POINT('Ctrl Pts',(6.94458082712411,287.423925943689,3.97163317015235));
#9384=CARTESIAN_POINT('Ctrl Pts',(5.88038492654913,287.561425943689,5.83242799455291));
#9385=CARTESIAN_POINT('Ctrl Pts',(4.02836682984766,287.698925943689,6.91182563342691));
#9386=CARTESIAN_POINT('Ctrl Pts',(2.17634873314619,287.836425943689,7.99122327230091));
#9387=CARTESIAN_POINT('Ctrl Pts',(0.0327551936971994,287.973925943689,8.));
#9388=CARTESIAN_POINT('Ctrl Pts',(-2.11083834575178,288.111425943689,8.00877672769909));
#9389=CARTESIAN_POINT('Ctrl Pts',(-3.97163317015234,288.248925943689,6.94458082712412));
#9390=CARTESIAN_POINT('Ctrl Pts',(-5.83242799455291,288.386425943689,5.88038492654913));
#9391=CARTESIAN_POINT('Ctrl Pts',(-6.91182563342691,288.523925943689,4.02836682984766));
#9392=CARTESIAN_POINT('Ctrl Pts',(-7.99122327230091,288.661425943689,2.17634873314619));
#9393=CARTESIAN_POINT('Ctrl Pts',(-8.,288.798925943689,0.0327551936971979));
#9394=CARTESIAN_POINT('Ctrl Pts',(-8.00877672769909,288.936425943689,-2.11083834575178));
#9395=CARTESIAN_POINT('Ctrl Pts',(-6.94458082712411,289.073925943689,-3.97163317015235));
#9396=CARTESIAN_POINT('Ctrl Pts',(-5.88038492654913,289.211425943689,-5.83242799455291));
#9397=CARTESIAN_POINT('Ctrl Pts',(-4.02836682984766,289.348925943689,-6.91182563342691));
#9398=CARTESIAN_POINT('Ctrl Pts',(-2.17634873314618,289.486425943689,-7.99122327230091));
#9399=CARTESIAN_POINT('Ctrl Pts',(-0.0327551936971984,289.623925943689,
-8.));
#9400=CARTESIAN_POINT('Ctrl Pts',(2.11083834575178,289.761425943689,-8.00877672769909));
#9401=CARTESIAN_POINT('Ctrl Pts',(3.97163317015235,289.898925943689,-6.94458082712411));
#9402=CARTESIAN_POINT('Ctrl Pts',(5.83242799455291,290.036425943689,-5.88038492654913));
#9403=CARTESIAN_POINT('Ctrl Pts',(6.91182563342691,290.173925943689,-4.02836682984766));
#9404=CARTESIAN_POINT('Ctrl Pts',(7.99122327230091,290.311425943689,-2.17634873314618));
#9405=CARTESIAN_POINT('Ctrl Pts',(8.,290.448925943689,-0.0327551936971989));
#9406=CARTESIAN_POINT('Ctrl Pts',(8.00877672769909,290.586425943689,2.11083834575178));
#9407=CARTESIAN_POINT('Ctrl Pts',(6.94458082712411,290.723925943689,3.97163317015235));
#9408=CARTESIAN_POINT('Ctrl Pts',(5.88038492654913,290.861425943689,5.83242799455291));
#9409=CARTESIAN_POINT('Ctrl Pts',(4.02836682984766,290.998925943689,6.91182563342691));
#9410=CARTESIAN_POINT('Ctrl Pts',(2.17634873314619,291.136425943689,7.99122327230091));
#9411=CARTESIAN_POINT('Ctrl Pts',(0.0327551936971994,291.273925943689,8.));
#9412=CARTESIAN_POINT('Ctrl Pts',(-2.11083834575178,291.411425943689,8.00877672769909));
#9413=CARTESIAN_POINT('Ctrl Pts',(-3.97163317015234,291.548925943689,6.94458082712412));
#9414=CARTESIAN_POINT('Ctrl Pts',(-5.83242799455291,291.686425943689,5.88038492654913));
#9415=CARTESIAN_POINT('Ctrl Pts',(-6.91182563342691,291.823925943689,4.02836682984766));
#9416=CARTESIAN_POINT('Ctrl Pts',(-7.99122327230091,291.961425943689,2.17634873314619));
#9417=CARTESIAN_POINT('Ctrl Pts',(-8.,292.098925943689,0.0327551936971979));
#9418=CARTESIAN_POINT('Ctrl Pts',(-8.00877672769909,292.236425943689,-2.11083834575178));
#9419=CARTESIAN_POINT('Ctrl Pts',(-6.94458082712411,292.373925943689,-3.97163317015235));
#9420=CARTESIAN_POINT('Ctrl Pts',(-5.88038492654913,292.511425943689,-5.83242799455291));
#9421=CARTESIAN_POINT('Ctrl Pts',(-4.02836682984766,292.648925943689,-6.91182563342691));
#9422=CARTESIAN_POINT('Ctrl Pts',(-2.17634873314618,292.786425943689,-7.99122327230091));
#9423=CARTESIAN_POINT('Ctrl Pts',(-0.0327551936971984,292.923925943689,
-8.));
#9424=CARTESIAN_POINT('Ctrl Pts',(2.11083834575178,293.061425943689,-8.00877672769909));
#9425=CARTESIAN_POINT('Ctrl Pts',(3.97163317015235,293.198925943689,-6.94458082712411));
#9426=CARTESIAN_POINT('Ctrl Pts',(5.83242799455291,293.336425943689,-5.88038492654913));
#9427=CARTESIAN_POINT('Ctrl Pts',(6.91182563342691,293.473925943689,-4.02836682984766));
#9428=CARTESIAN_POINT('Ctrl Pts',(7.99122327230091,293.611425943689,-2.17634873314618));
#9429=CARTESIAN_POINT('Ctrl Pts',(8.,293.748925943689,-0.0327551936971989));
#9430=CARTESIAN_POINT('Ctrl Pts',(8.00877672769909,293.886425943689,2.11083834575178));
#9431=CARTESIAN_POINT('Ctrl Pts',(6.94458082712411,294.023925943689,3.97163317015235));
#9432=CARTESIAN_POINT('Ctrl Pts',(5.88038492654913,294.161425943689,5.83242799455291));
#9433=CARTESIAN_POINT('Ctrl Pts',(4.02836682984766,294.298925943689,6.91182563342691));
#9434=CARTESIAN_POINT('Ctrl Pts',(2.17634873314619,294.436425943689,7.99122327230091));
#9435=CARTESIAN_POINT('Ctrl Pts',(0.0327551936971994,294.573925943689,8.));
#9436=CARTESIAN_POINT('Ctrl Pts',(-2.11083834575178,294.711425943689,8.00877672769909));
#9437=CARTESIAN_POINT('Ctrl Pts',(-3.97163317015234,294.848925943689,6.94458082712412));
#9438=CARTESIAN_POINT('Ctrl Pts',(-5.83242799455291,294.986425943689,5.88038492654913));
#9439=CARTESIAN_POINT('Ctrl Pts',(-6.91182563342691,295.123925943689,4.02836682984766));
#9440=CARTESIAN_POINT('Ctrl Pts',(-7.99122327230091,295.261425943689,2.17634873314619));
#9441=CARTESIAN_POINT('Ctrl Pts',(-8.,295.398925943689,0.0327551936971979));
#9442=CARTESIAN_POINT('Ctrl Pts',(-8.00877672769909,295.536425943689,-2.11083834575178));
#9443=CARTESIAN_POINT('Ctrl Pts',(-6.94458082712411,295.673925943689,-3.97163317015235));
#9444=CARTESIAN_POINT('Ctrl Pts',(-5.88038492654913,295.811425943689,-5.83242799455291));
#9445=CARTESIAN_POINT('Ctrl Pts',(-4.02836682984766,295.948925943689,-6.91182563342691));
#9446=CARTESIAN_POINT('Ctrl Pts',(-2.17634873314618,296.086425943689,-7.99122327230091));
#9447=CARTESIAN_POINT('Ctrl Pts',(-0.0327551936971984,296.223925943689,
-8.));
#9448=CARTESIAN_POINT('Ctrl Pts',(2.11083834575178,296.361425943689,-8.00877672769909));
#9449=CARTESIAN_POINT('Ctrl Pts',(3.97163317015235,296.498925943689,-6.94458082712411));
#9450=CARTESIAN_POINT('Ctrl Pts',(5.83242799455291,296.636425943689,-5.88038492654913));
#9451=CARTESIAN_POINT('Ctrl Pts',(6.91182563342691,296.773925943689,-4.02836682984766));
#9452=CARTESIAN_POINT('Ctrl Pts',(7.99122327230091,296.911425943689,-2.17634873314618));
#9453=CARTESIAN_POINT('Ctrl Pts',(8.,297.048925943689,-0.0327551936971989));
#9454=CARTESIAN_POINT('Ctrl Pts',(8.00877672769909,297.186425943689,2.11083834575178));
#9455=CARTESIAN_POINT('Ctrl Pts',(6.94458082712411,297.323925943689,3.97163317015235));
#9456=CARTESIAN_POINT('Ctrl Pts',(5.88038492654913,297.461425943689,5.83242799455291));
#9457=CARTESIAN_POINT('Ctrl Pts',(4.02836682984766,297.598925943689,6.91182563342691));
#9458=CARTESIAN_POINT('Ctrl Pts',(2.17634873314619,297.736425943689,7.99122327230091));
#9459=CARTESIAN_POINT('Ctrl Pts',(0.0327551936971994,297.873925943689,8.));
#9460=CARTESIAN_POINT('Ctrl Pts',(-2.11083834575178,298.011425943689,8.00877672769909));
#9461=CARTESIAN_POINT('Ctrl Pts',(-3.97163317015234,298.148925943689,6.94458082712412));
#9462=CARTESIAN_POINT('Ctrl Pts',(-5.83242799455291,298.286425943689,5.88038492654913));
#9463=CARTESIAN_POINT('Ctrl Pts',(-6.91182563342691,298.423925943689,4.02836682984766));
#9464=CARTESIAN_POINT('Ctrl Pts',(-7.99122327230091,298.561425943689,2.17634873314619));
#9465=CARTESIAN_POINT('Ctrl Pts',(-8.,298.698925943689,0.0327551936971979));
#9466=CARTESIAN_POINT('Ctrl Pts',(-8.00877672769909,298.836425943689,-2.11083834575178));
#9467=CARTESIAN_POINT('Ctrl Pts',(-6.94458082712411,298.973925943689,-3.97163317015235));
#9468=CARTESIAN_POINT('Ctrl Pts',(-5.88038492654913,299.111425943689,-5.83242799455291));
#9469=CARTESIAN_POINT('Ctrl Pts',(-4.02836682984766,299.248925943689,-6.91182563342691));
#9470=CARTESIAN_POINT('Ctrl Pts',(-2.17634873314618,299.386425943689,-7.99122327230091));
#9471=CARTESIAN_POINT('Ctrl Pts',(-0.0327551936971984,299.523925943689,
-8.));
#9472=CARTESIAN_POINT('Ctrl Pts',(2.11083834575178,299.661425943689,-8.00877672769909));
#9473=CARTESIAN_POINT('Ctrl Pts',(3.97163317015235,299.798925943689,-6.94458082712411));
#9474=CARTESIAN_POINT('Ctrl Pts',(5.83242799455291,299.936425943689,-5.88038492654913));
#9475=CARTESIAN_POINT('Ctrl Pts',(6.91182563342691,300.073925943689,-4.02836682984766));
#9476=CARTESIAN_POINT('Ctrl Pts',(7.99122327230091,300.211425943689,-2.17634873314618));
#9477=CARTESIAN_POINT('Ctrl Pts',(8.,300.348925943689,-0.0327551936971989));
#9478=CARTESIAN_POINT('Ctrl Pts',(8.00877672769909,300.486425943689,2.11083834575178));
#9479=CARTESIAN_POINT('Ctrl Pts',(6.94458082712411,300.623925943689,3.97163317015235));
#9480=CARTESIAN_POINT('Ctrl Pts',(5.88038492654913,300.761425943689,5.83242799455291));
#9481=CARTESIAN_POINT('Ctrl Pts',(4.02836682984766,300.898925943689,6.91182563342691));
#9482=CARTESIAN_POINT('Ctrl Pts',(2.17634873314619,301.036425943689,7.99122327230091));
#9483=CARTESIAN_POINT('Ctrl Pts',(0.0327551936971994,301.173925943689,8.));
#9484=CARTESIAN_POINT('Ctrl Pts',(-2.11083834575178,301.311425943689,8.00877672769909));
#9485=CARTESIAN_POINT('Ctrl Pts',(-3.97163317015234,301.448925943689,6.94458082712412));
#9486=CARTESIAN_POINT('Ctrl Pts',(-5.83242799455291,301.586425943689,5.88038492654913));
#9487=CARTESIAN_POINT('Ctrl Pts',(-6.91182563342691,301.723925943689,4.02836682984766));
#9488=CARTESIAN_POINT('Ctrl Pts',(-7.99122327230091,301.861425943689,2.17634873314619));
#9489=CARTESIAN_POINT('Ctrl Pts',(-8.,301.998925943689,0.0327551936971979));
#9490=CARTESIAN_POINT('Ctrl Pts',(-8.00877672769909,302.136425943689,-2.11083834575178));
#9491=CARTESIAN_POINT('Ctrl Pts',(-6.94458082712411,302.273925943689,-3.97163317015235));
#9492=CARTESIAN_POINT('Ctrl Pts',(-5.88038492654913,302.411425943689,-5.83242799455291));
#9493=CARTESIAN_POINT('Ctrl Pts',(-4.02836682984766,302.548925943689,-6.91182563342691));
#9494=CARTESIAN_POINT('Ctrl Pts',(-2.17634873314618,302.686425943689,-7.99122327230091));
#9495=CARTESIAN_POINT('Ctrl Pts',(-0.0327551936971984,302.823925943689,
-8.));
#9496=CARTESIAN_POINT('Ctrl Pts',(2.11083834575178,302.961425943689,-8.00877672769909));
#9497=CARTESIAN_POINT('Ctrl Pts',(3.97163317015235,303.098925943689,-6.94458082712411));
#9498=CARTESIAN_POINT('Ctrl Pts',(5.83242799455291,303.236425943689,-5.88038492654913));
#9499=CARTESIAN_POINT('Ctrl Pts',(6.91182563342691,303.373925943689,-4.02836682984766));
#9500=CARTESIAN_POINT('Ctrl Pts',(7.99122327230091,303.511425943689,-2.17634873314618));
#9501=CARTESIAN_POINT('Ctrl Pts',(8.,303.648925943689,-0.0327551936971989));
#9502=CARTESIAN_POINT('Ctrl Pts',(8.00877672769909,303.786425943689,2.11083834575178));
#9503=CARTESIAN_POINT('Ctrl Pts',(6.94458082712411,303.923925943689,3.97163317015235));
#9504=CARTESIAN_POINT('Ctrl Pts',(5.88038492654913,304.061425943689,5.83242799455291));
#9505=CARTESIAN_POINT('Ctrl Pts',(4.02836682984766,304.198925943689,6.91182563342691));
#9506=CARTESIAN_POINT('Ctrl Pts',(2.17634873314619,304.336425943689,7.99122327230091));
#9507=CARTESIAN_POINT('Ctrl Pts',(0.0327551936971994,304.473925943689,8.));
#9508=CARTESIAN_POINT('Ctrl Pts',(-2.11083834575178,304.611425943689,8.00877672769909));
#9509=CARTESIAN_POINT('Ctrl Pts',(-3.97163317015234,304.748925943689,6.94458082712412));
#9510=CARTESIAN_POINT('Ctrl Pts',(-5.83242799455291,304.886425943689,5.88038492654913));
#9511=CARTESIAN_POINT('Ctrl Pts',(-6.91182563342691,305.023925943689,4.02836682984766));
#9512=CARTESIAN_POINT('Ctrl Pts',(-7.99122327230091,305.161425943689,2.17634873314619));
#9513=CARTESIAN_POINT('Ctrl Pts',(-8.,305.298925943689,0.0327551936971979));
#9514=CARTESIAN_POINT('Ctrl Pts',(-8.00877672769909,305.436425943689,-2.11083834575178));
#9515=CARTESIAN_POINT('Ctrl Pts',(-6.94458082712411,305.573925943689,-3.97163317015235));
#9516=CARTESIAN_POINT('Ctrl Pts',(-5.88038492654913,305.711425943689,-5.83242799455291));
#9517=CARTESIAN_POINT('Ctrl Pts',(-4.02836682984766,305.848925943689,-6.91182563342691));
#9518=CARTESIAN_POINT('Ctrl Pts',(-2.17634873314618,305.986425943689,-7.99122327230091));
#9519=CARTESIAN_POINT('Ctrl Pts',(-0.0327551936971984,306.123925943689,
-8.));
#9520=CARTESIAN_POINT('Ctrl Pts',(2.11083834575178,306.261425943689,-8.00877672769909));
#9521=CARTESIAN_POINT('Ctrl Pts',(3.97163317015235,306.398925943689,-6.94458082712411));
#9522=CARTESIAN_POINT('Ctrl Pts',(5.83242799455291,306.536425943689,-5.88038492654913));
#9523=CARTESIAN_POINT('Ctrl Pts',(6.91182563342691,306.673925943689,-4.02836682984766));
#9524=CARTESIAN_POINT('Ctrl Pts',(7.99122327230091,306.811425943689,-2.17634873314618));
#9525=CARTESIAN_POINT('Ctrl Pts',(8.,306.948925943689,-0.0327551936971989));
#9526=CARTESIAN_POINT('Ctrl Pts',(8.00877672769909,307.086425943689,2.11083834575178));
#9527=CARTESIAN_POINT('Ctrl Pts',(6.94458082712411,307.223925943689,3.97163317015235));
#9528=CARTESIAN_POINT('Ctrl Pts',(5.88038492654913,307.361425943689,5.83242799455291));
#9529=CARTESIAN_POINT('Ctrl Pts',(4.02836682984766,307.498925943689,6.91182563342691));
#9530=CARTESIAN_POINT('Ctrl Pts',(2.17634873314619,307.636425943689,7.99122327230091));
#9531=CARTESIAN_POINT('Ctrl Pts',(0.0327551936971994,307.773925943689,8.));
#9532=CARTESIAN_POINT('Ctrl Pts',(-2.11083834575178,307.911425943689,8.00877672769909));
#9533=CARTESIAN_POINT('Ctrl Pts',(-3.97163317015234,308.048925943689,6.94458082712412));
#9534=CARTESIAN_POINT('Ctrl Pts',(-5.83242799455291,308.186425943689,5.88038492654913));
#9535=CARTESIAN_POINT('Ctrl Pts',(-6.91182563342691,308.323925943689,4.02836682984766));
#9536=CARTESIAN_POINT('Ctrl Pts',(-7.99122327230091,308.461425943689,2.17634873314619));
#9537=CARTESIAN_POINT('Ctrl Pts',(-8.,308.598925943689,0.0327551936971979));
#9538=CARTESIAN_POINT('Ctrl Pts',(-8.00877672769909,308.736425943689,-2.11083834575178));
#9539=CARTESIAN_POINT('Ctrl Pts',(-6.94458082712411,308.873925943689,-3.97163317015235));
#9540=CARTESIAN_POINT('Ctrl Pts',(-5.88038492654913,309.011425943689,-5.83242799455291));
#9541=CARTESIAN_POINT('Ctrl Pts',(-4.02836682984766,309.148925943689,-6.91182563342691));
#9542=CARTESIAN_POINT('Ctrl Pts',(-2.17634873314618,309.286425943689,-7.99122327230091));
#9543=CARTESIAN_POINT('Ctrl Pts',(-0.0327551936971984,309.423925943689,
-8.));
#9544=CARTESIAN_POINT('Ctrl Pts',(2.11083834575178,309.561425943689,-8.00877672769909));
#9545=CARTESIAN_POINT('Ctrl Pts',(3.97163317015235,309.698925943689,-6.94458082712411));
#9546=CARTESIAN_POINT('Ctrl Pts',(5.83242799455291,309.836425943689,-5.88038492654913));
#9547=CARTESIAN_POINT('Ctrl Pts',(6.91182563342691,309.973925943689,-4.02836682984766));
#9548=CARTESIAN_POINT('Ctrl Pts',(7.99122327230091,310.111425943689,-2.17634873314618));
#9549=CARTESIAN_POINT('Ctrl Pts',(8.,310.248925943689,-0.0327551936971989));
#9550=CARTESIAN_POINT('Ctrl Pts',(8.00877672769909,310.386425943689,2.11083834575178));
#9551=CARTESIAN_POINT('Ctrl Pts',(6.94458082712411,310.523925943689,3.97163317015235));
#9552=CARTESIAN_POINT('Ctrl Pts',(5.88038492654913,310.661425943689,5.83242799455291));
#9553=CARTESIAN_POINT('Ctrl Pts',(4.02836682984766,310.798925943689,6.91182563342691));
#9554=CARTESIAN_POINT('Ctrl Pts',(2.17634873314619,310.936425943689,7.99122327230091));
#9555=CARTESIAN_POINT('Ctrl Pts',(0.0327551936971994,311.073925943689,8.));
#9556=CARTESIAN_POINT('Ctrl Pts',(-2.11083834575178,311.211425943689,8.00877672769909));
#9557=CARTESIAN_POINT('Ctrl Pts',(-3.97163317015234,311.348925943689,6.94458082712412));
#9558=CARTESIAN_POINT('Ctrl Pts',(-5.83242799455291,311.486425943689,5.88038492654913));
#9559=CARTESIAN_POINT('Ctrl Pts',(-6.91182563342691,311.623925943689,4.02836682984766));
#9560=CARTESIAN_POINT('Ctrl Pts',(-7.99122327230091,311.761425943689,2.17634873314619));
#9561=CARTESIAN_POINT('Ctrl Pts',(-8.,311.898925943689,0.0327551936971979));
#9562=CARTESIAN_POINT('Ctrl Pts',(-8.00877672769909,312.036425943689,-2.11083834575178));
#9563=CARTESIAN_POINT('Ctrl Pts',(-6.94458082712411,312.173925943689,-3.97163317015235));
#9564=CARTESIAN_POINT('Ctrl Pts',(-5.88038492654913,312.311425943689,-5.83242799455291));
#9565=CARTESIAN_POINT('Ctrl Pts',(-4.02836682984766,312.448925943689,-6.91182563342691));
#9566=CARTESIAN_POINT('Ctrl Pts',(-2.17634873314618,312.586425943689,-7.99122327230091));
#9567=CARTESIAN_POINT('Ctrl Pts',(-0.0327551936971984,312.723925943689,
-8.));
#9568=CARTESIAN_POINT('Ctrl Pts',(2.11083834575178,312.861425943689,-8.00877672769909));
#9569=CARTESIAN_POINT('Ctrl Pts',(3.97163317015235,312.998925943689,-6.94458082712411));
#9570=CARTESIAN_POINT('Ctrl Pts',(5.83242799455291,313.136425943689,-5.88038492654913));
#9571=CARTESIAN_POINT('Ctrl Pts',(6.91182563342691,313.273925943689,-4.02836682984766));
#9572=CARTESIAN_POINT('Ctrl Pts',(7.99122327230091,313.411425943689,-2.17634873314618));
#9573=CARTESIAN_POINT('Ctrl Pts',(8.,313.548925943689,-0.0327551936971989));
#9574=CARTESIAN_POINT('Ctrl Pts',(8.00877672769909,313.686425943689,2.11083834575178));
#9575=CARTESIAN_POINT('Ctrl Pts',(6.94458082712411,313.823925943689,3.97163317015235));
#9576=CARTESIAN_POINT('Ctrl Pts',(5.88038492654913,313.961425943689,5.83242799455291));
#9577=CARTESIAN_POINT('Ctrl Pts',(4.02836682984766,314.098925943689,6.91182563342691));
#9578=CARTESIAN_POINT('Ctrl Pts',(2.17634873314619,314.236425943689,7.99122327230091));
#9579=CARTESIAN_POINT('Ctrl Pts',(0.0327551936971994,314.373925943689,8.));
#9580=CARTESIAN_POINT('Ctrl Pts',(-2.11083834575178,314.511425943689,8.00877672769909));
#9581=CARTESIAN_POINT('Ctrl Pts',(-3.97163317015234,314.648925943689,6.94458082712412));
#9582=CARTESIAN_POINT('Ctrl Pts',(-5.83242799455291,314.786425943689,5.88038492654913));
#9583=CARTESIAN_POINT('Ctrl Pts',(-6.91182563342691,314.923925943689,4.02836682984766));
#9584=CARTESIAN_POINT('Ctrl Pts',(-7.99122327230091,315.061425943689,2.17634873314619));
#9585=CARTESIAN_POINT('Ctrl Pts',(-8.,315.198925943689,0.0327551936971979));
#9586=CARTESIAN_POINT('Ctrl Pts',(-8.00877672769909,315.336425943689,-2.11083834575178));
#9587=CARTESIAN_POINT('Ctrl Pts',(-6.94458082712411,315.473925943689,-3.97163317015235));
#9588=CARTESIAN_POINT('Ctrl Pts',(-5.88038492654913,315.611425943689,-5.83242799455291));
#9589=CARTESIAN_POINT('Ctrl Pts',(-4.02836682984766,315.748925943689,-6.91182563342691));
#9590=CARTESIAN_POINT('Ctrl Pts',(-2.17634873314618,315.886425943689,-7.99122327230091));
#9591=CARTESIAN_POINT('Ctrl Pts',(-0.0327551936971984,316.023925943689,
-8.));
#9592=CARTESIAN_POINT('Ctrl Pts',(2.11083834575178,316.161425943689,-8.00877672769909));
#9593=CARTESIAN_POINT('Ctrl Pts',(3.97163317015235,316.298925943689,-6.94458082712411));
#9594=CARTESIAN_POINT('Ctrl Pts',(5.83242799455291,316.436425943689,-5.88038492654913));
#9595=CARTESIAN_POINT('Ctrl Pts',(6.91182563342691,316.573925943689,-4.02836682984766));
#9596=CARTESIAN_POINT('Ctrl Pts',(7.99122327230091,316.711425943689,-2.17634873314618));
#9597=CARTESIAN_POINT('Ctrl Pts',(8.,316.848925943689,-0.0327551936971989));
#9598=CARTESIAN_POINT('Ctrl Pts',(8.00877672769909,316.986425943689,2.11083834575178));
#9599=CARTESIAN_POINT('Ctrl Pts',(6.94458082712411,317.123925943689,3.97163317015235));
#9600=CARTESIAN_POINT('Ctrl Pts',(5.88038492654913,317.261425943689,5.83242799455291));
#9601=CARTESIAN_POINT('Ctrl Pts',(4.02836682984766,317.398925943689,6.91182563342691));
#9602=CARTESIAN_POINT('Ctrl Pts',(2.17634873314619,317.536425943689,7.99122327230091));
#9603=CARTESIAN_POINT('Ctrl Pts',(0.0327551936971994,317.673925943689,8.));
#9604=CARTESIAN_POINT('Ctrl Pts',(-2.11083834575178,317.811425943689,8.00877672769909));
#9605=CARTESIAN_POINT('Ctrl Pts',(-3.97163317015234,317.948925943689,6.94458082712412));
#9606=CARTESIAN_POINT('Ctrl Pts',(-5.83242799455291,318.086425943689,5.88038492654913));
#9607=CARTESIAN_POINT('Ctrl Pts',(-6.91182563342691,318.223925943689,4.02836682984766));
#9608=CARTESIAN_POINT('Ctrl Pts',(-7.99122327230091,318.361425943689,2.17634873314619));
#9609=CARTESIAN_POINT('Ctrl Pts',(-8.,318.498925943689,0.0327551936971979));
#9610=CARTESIAN_POINT('Ctrl Pts',(-7.,285.498925943689,0.0327551936971879));
#9611=CARTESIAN_POINT('Ctrl Pts',(-7.00877672769909,285.636425943689,-1.84288915332067));
#9612=CARTESIAN_POINT('Ctrl Pts',(-6.07855542333967,285.773925943689,-3.47163317015236));
#9613=CARTESIAN_POINT('Ctrl Pts',(-5.14833411898024,285.911425943689,-5.10037718698404));
#9614=CARTESIAN_POINT('Ctrl Pts',(-3.52836682984765,286.048925943689,-6.04580022964248));
#9615=CARTESIAN_POINT('Ctrl Pts',(-1.90839954071505,286.186425943689,-6.99122327230092));
#9616=CARTESIAN_POINT('Ctrl Pts',(-0.0327551936971884,286.323925943689,
-7.));
#9617=CARTESIAN_POINT('Ctrl Pts',(1.84288915332067,286.461425943689,-7.00877672769909));
#9618=CARTESIAN_POINT('Ctrl Pts',(3.47163317015236,286.598925943689,-6.07855542333967));
#9619=CARTESIAN_POINT('Ctrl Pts',(5.10037718698404,286.736425943689,-5.14833411898024));
#9620=CARTESIAN_POINT('Ctrl Pts',(6.04580022964248,286.873925943689,-3.52836682984765));
#9621=CARTESIAN_POINT('Ctrl Pts',(6.99122327230092,287.011425943689,-1.90839954071505));
#9622=CARTESIAN_POINT('Ctrl Pts',(7.,287.148925943689,-0.0327551936971888));
#9623=CARTESIAN_POINT('Ctrl Pts',(7.00877672769909,287.286425943689,1.84288915332067));
#9624=CARTESIAN_POINT('Ctrl Pts',(6.07855542333967,287.423925943689,3.47163317015236));
#9625=CARTESIAN_POINT('Ctrl Pts',(5.14833411898025,287.561425943689,5.10037718698404));
#9626=CARTESIAN_POINT('Ctrl Pts',(3.52836682984765,287.698925943689,6.04580022964248));
#9627=CARTESIAN_POINT('Ctrl Pts',(1.90839954071505,287.836425943689,6.99122327230091));
#9628=CARTESIAN_POINT('Ctrl Pts',(0.0327551936971892,287.973925943689,7.));
#9629=CARTESIAN_POINT('Ctrl Pts',(-1.84288915332067,288.111425943689,7.00877672769909));
#9630=CARTESIAN_POINT('Ctrl Pts',(-3.47163317015235,288.248925943689,6.07855542333967));
#9631=CARTESIAN_POINT('Ctrl Pts',(-5.10037718698404,288.386425943689,5.14833411898025));
#9632=CARTESIAN_POINT('Ctrl Pts',(-6.04580022964248,288.523925943689,3.52836682984765));
#9633=CARTESIAN_POINT('Ctrl Pts',(-6.99122327230091,288.661425943689,1.90839954071505));
#9634=CARTESIAN_POINT('Ctrl Pts',(-7.,288.798925943689,0.0327551936971879));
#9635=CARTESIAN_POINT('Ctrl Pts',(-7.00877672769909,288.936425943689,-1.84288915332067));
#9636=CARTESIAN_POINT('Ctrl Pts',(-6.07855542333967,289.073925943689,-3.47163317015236));
#9637=CARTESIAN_POINT('Ctrl Pts',(-5.14833411898024,289.211425943689,-5.10037718698404));
#9638=CARTESIAN_POINT('Ctrl Pts',(-3.52836682984765,289.348925943689,-6.04580022964248));
#9639=CARTESIAN_POINT('Ctrl Pts',(-1.90839954071505,289.486425943689,-6.99122327230092));
#9640=CARTESIAN_POINT('Ctrl Pts',(-0.0327551936971884,289.623925943689,
-7.));
#9641=CARTESIAN_POINT('Ctrl Pts',(1.84288915332067,289.761425943689,-7.00877672769909));
#9642=CARTESIAN_POINT('Ctrl Pts',(3.47163317015236,289.898925943689,-6.07855542333967));
#9643=CARTESIAN_POINT('Ctrl Pts',(5.10037718698404,290.036425943689,-5.14833411898024));
#9644=CARTESIAN_POINT('Ctrl Pts',(6.04580022964248,290.173925943689,-3.52836682984765));
#9645=CARTESIAN_POINT('Ctrl Pts',(6.99122327230092,290.311425943689,-1.90839954071505));
#9646=CARTESIAN_POINT('Ctrl Pts',(7.,290.448925943689,-0.0327551936971888));
#9647=CARTESIAN_POINT('Ctrl Pts',(7.00877672769909,290.586425943689,1.84288915332067));
#9648=CARTESIAN_POINT('Ctrl Pts',(6.07855542333967,290.723925943689,3.47163317015236));
#9649=CARTESIAN_POINT('Ctrl Pts',(5.14833411898025,290.861425943689,5.10037718698404));
#9650=CARTESIAN_POINT('Ctrl Pts',(3.52836682984765,290.998925943689,6.04580022964248));
#9651=CARTESIAN_POINT('Ctrl Pts',(1.90839954071505,291.136425943689,6.99122327230091));
#9652=CARTESIAN_POINT('Ctrl Pts',(0.0327551936971892,291.273925943689,7.));
#9653=CARTESIAN_POINT('Ctrl Pts',(-1.84288915332067,291.411425943689,7.00877672769909));
#9654=CARTESIAN_POINT('Ctrl Pts',(-3.47163317015235,291.548925943689,6.07855542333967));
#9655=CARTESIAN_POINT('Ctrl Pts',(-5.10037718698404,291.686425943689,5.14833411898025));
#9656=CARTESIAN_POINT('Ctrl Pts',(-6.04580022964248,291.823925943689,3.52836682984765));
#9657=CARTESIAN_POINT('Ctrl Pts',(-6.99122327230091,291.961425943689,1.90839954071505));
#9658=CARTESIAN_POINT('Ctrl Pts',(-7.,292.098925943689,0.0327551936971879));
#9659=CARTESIAN_POINT('Ctrl Pts',(-7.00877672769909,292.236425943689,-1.84288915332067));
#9660=CARTESIAN_POINT('Ctrl Pts',(-6.07855542333967,292.373925943689,-3.47163317015236));
#9661=CARTESIAN_POINT('Ctrl Pts',(-5.14833411898024,292.511425943689,-5.10037718698404));
#9662=CARTESIAN_POINT('Ctrl Pts',(-3.52836682984765,292.648925943689,-6.04580022964248));
#9663=CARTESIAN_POINT('Ctrl Pts',(-1.90839954071505,292.786425943689,-6.99122327230092));
#9664=CARTESIAN_POINT('Ctrl Pts',(-0.0327551936971884,292.923925943689,
-7.));
#9665=CARTESIAN_POINT('Ctrl Pts',(1.84288915332067,293.061425943689,-7.00877672769909));
#9666=CARTESIAN_POINT('Ctrl Pts',(3.47163317015236,293.198925943689,-6.07855542333967));
#9667=CARTESIAN_POINT('Ctrl Pts',(5.10037718698404,293.336425943689,-5.14833411898024));
#9668=CARTESIAN_POINT('Ctrl Pts',(6.04580022964248,293.473925943689,-3.52836682984765));
#9669=CARTESIAN_POINT('Ctrl Pts',(6.99122327230092,293.611425943689,-1.90839954071505));
#9670=CARTESIAN_POINT('Ctrl Pts',(7.,293.748925943689,-0.0327551936971888));
#9671=CARTESIAN_POINT('Ctrl Pts',(7.00877672769909,293.886425943689,1.84288915332067));
#9672=CARTESIAN_POINT('Ctrl Pts',(6.07855542333967,294.023925943689,3.47163317015236));
#9673=CARTESIAN_POINT('Ctrl Pts',(5.14833411898025,294.161425943689,5.10037718698404));
#9674=CARTESIAN_POINT('Ctrl Pts',(3.52836682984765,294.298925943689,6.04580022964248));
#9675=CARTESIAN_POINT('Ctrl Pts',(1.90839954071505,294.436425943689,6.99122327230091));
#9676=CARTESIAN_POINT('Ctrl Pts',(0.0327551936971892,294.573925943689,7.));
#9677=CARTESIAN_POINT('Ctrl Pts',(-1.84288915332067,294.711425943689,7.00877672769909));
#9678=CARTESIAN_POINT('Ctrl Pts',(-3.47163317015235,294.848925943689,6.07855542333967));
#9679=CARTESIAN_POINT('Ctrl Pts',(-5.10037718698404,294.986425943689,5.14833411898025));
#9680=CARTESIAN_POINT('Ctrl Pts',(-6.04580022964248,295.123925943689,3.52836682984765));
#9681=CARTESIAN_POINT('Ctrl Pts',(-6.99122327230091,295.261425943689,1.90839954071505));
#9682=CARTESIAN_POINT('Ctrl Pts',(-7.,295.398925943689,0.0327551936971879));
#9683=CARTESIAN_POINT('Ctrl Pts',(-7.00877672769909,295.536425943689,-1.84288915332067));
#9684=CARTESIAN_POINT('Ctrl Pts',(-6.07855542333967,295.673925943689,-3.47163317015236));
#9685=CARTESIAN_POINT('Ctrl Pts',(-5.14833411898024,295.811425943689,-5.10037718698404));
#9686=CARTESIAN_POINT('Ctrl Pts',(-3.52836682984765,295.948925943689,-6.04580022964248));
#9687=CARTESIAN_POINT('Ctrl Pts',(-1.90839954071505,296.086425943689,-6.99122327230092));
#9688=CARTESIAN_POINT('Ctrl Pts',(-0.0327551936971884,296.223925943689,
-7.));
#9689=CARTESIAN_POINT('Ctrl Pts',(1.84288915332067,296.361425943689,-7.00877672769909));
#9690=CARTESIAN_POINT('Ctrl Pts',(3.47163317015236,296.498925943689,-6.07855542333967));
#9691=CARTESIAN_POINT('Ctrl Pts',(5.10037718698404,296.636425943689,-5.14833411898024));
#9692=CARTESIAN_POINT('Ctrl Pts',(6.04580022964248,296.773925943689,-3.52836682984765));
#9693=CARTESIAN_POINT('Ctrl Pts',(6.99122327230092,296.911425943689,-1.90839954071505));
#9694=CARTESIAN_POINT('Ctrl Pts',(7.,297.048925943689,-0.0327551936971888));
#9695=CARTESIAN_POINT('Ctrl Pts',(7.00877672769909,297.186425943689,1.84288915332067));
#9696=CARTESIAN_POINT('Ctrl Pts',(6.07855542333967,297.323925943689,3.47163317015236));
#9697=CARTESIAN_POINT('Ctrl Pts',(5.14833411898025,297.461425943689,5.10037718698404));
#9698=CARTESIAN_POINT('Ctrl Pts',(3.52836682984765,297.598925943689,6.04580022964248));
#9699=CARTESIAN_POINT('Ctrl Pts',(1.90839954071505,297.736425943689,6.99122327230091));
#9700=CARTESIAN_POINT('Ctrl Pts',(0.0327551936971892,297.873925943689,7.));
#9701=CARTESIAN_POINT('Ctrl Pts',(-1.84288915332067,298.011425943689,7.00877672769909));
#9702=CARTESIAN_POINT('Ctrl Pts',(-3.47163317015235,298.148925943689,6.07855542333967));
#9703=CARTESIAN_POINT('Ctrl Pts',(-5.10037718698404,298.286425943689,5.14833411898025));
#9704=CARTESIAN_POINT('Ctrl Pts',(-6.04580022964248,298.423925943689,3.52836682984765));
#9705=CARTESIAN_POINT('Ctrl Pts',(-6.99122327230091,298.561425943689,1.90839954071505));
#9706=CARTESIAN_POINT('Ctrl Pts',(-7.,298.698925943689,0.0327551936971879));
#9707=CARTESIAN_POINT('Ctrl Pts',(-7.00877672769909,298.836425943689,-1.84288915332067));
#9708=CARTESIAN_POINT('Ctrl Pts',(-6.07855542333967,298.973925943689,-3.47163317015236));
#9709=CARTESIAN_POINT('Ctrl Pts',(-5.14833411898024,299.111425943689,-5.10037718698404));
#9710=CARTESIAN_POINT('Ctrl Pts',(-3.52836682984765,299.248925943689,-6.04580022964248));
#9711=CARTESIAN_POINT('Ctrl Pts',(-1.90839954071505,299.386425943689,-6.99122327230092));
#9712=CARTESIAN_POINT('Ctrl Pts',(-0.0327551936971884,299.523925943689,
-7.));
#9713=CARTESIAN_POINT('Ctrl Pts',(1.84288915332067,299.661425943689,-7.00877672769909));
#9714=CARTESIAN_POINT('Ctrl Pts',(3.47163317015236,299.798925943689,-6.07855542333967));
#9715=CARTESIAN_POINT('Ctrl Pts',(5.10037718698404,299.936425943689,-5.14833411898024));
#9716=CARTESIAN_POINT('Ctrl Pts',(6.04580022964248,300.073925943689,-3.52836682984765));
#9717=CARTESIAN_POINT('Ctrl Pts',(6.99122327230092,300.211425943689,-1.90839954071505));
#9718=CARTESIAN_POINT('Ctrl Pts',(7.,300.348925943689,-0.0327551936971888));
#9719=CARTESIAN_POINT('Ctrl Pts',(7.00877672769909,300.486425943689,1.84288915332067));
#9720=CARTESIAN_POINT('Ctrl Pts',(6.07855542333967,300.623925943689,3.47163317015236));
#9721=CARTESIAN_POINT('Ctrl Pts',(5.14833411898025,300.761425943689,5.10037718698404));
#9722=CARTESIAN_POINT('Ctrl Pts',(3.52836682984765,300.898925943689,6.04580022964248));
#9723=CARTESIAN_POINT('Ctrl Pts',(1.90839954071505,301.036425943689,6.99122327230091));
#9724=CARTESIAN_POINT('Ctrl Pts',(0.0327551936971892,301.173925943689,7.));
#9725=CARTESIAN_POINT('Ctrl Pts',(-1.84288915332067,301.311425943689,7.00877672769909));
#9726=CARTESIAN_POINT('Ctrl Pts',(-3.47163317015235,301.448925943689,6.07855542333967));
#9727=CARTESIAN_POINT('Ctrl Pts',(-5.10037718698404,301.586425943689,5.14833411898025));
#9728=CARTESIAN_POINT('Ctrl Pts',(-6.04580022964248,301.723925943689,3.52836682984765));
#9729=CARTESIAN_POINT('Ctrl Pts',(-6.99122327230091,301.861425943689,1.90839954071505));
#9730=CARTESIAN_POINT('Ctrl Pts',(-7.,301.998925943689,0.0327551936971879));
#9731=CARTESIAN_POINT('Ctrl Pts',(-7.00877672769909,302.136425943689,-1.84288915332067));
#9732=CARTESIAN_POINT('Ctrl Pts',(-6.07855542333967,302.273925943689,-3.47163317015236));
#9733=CARTESIAN_POINT('Ctrl Pts',(-5.14833411898024,302.411425943689,-5.10037718698404));
#9734=CARTESIAN_POINT('Ctrl Pts',(-3.52836682984765,302.548925943689,-6.04580022964248));
#9735=CARTESIAN_POINT('Ctrl Pts',(-1.90839954071505,302.686425943689,-6.99122327230092));
#9736=CARTESIAN_POINT('Ctrl Pts',(-0.0327551936971884,302.823925943689,
-7.));
#9737=CARTESIAN_POINT('Ctrl Pts',(1.84288915332067,302.961425943689,-7.00877672769909));
#9738=CARTESIAN_POINT('Ctrl Pts',(3.47163317015236,303.098925943689,-6.07855542333967));
#9739=CARTESIAN_POINT('Ctrl Pts',(5.10037718698404,303.236425943689,-5.14833411898024));
#9740=CARTESIAN_POINT('Ctrl Pts',(6.04580022964248,303.373925943689,-3.52836682984765));
#9741=CARTESIAN_POINT('Ctrl Pts',(6.99122327230092,303.511425943689,-1.90839954071505));
#9742=CARTESIAN_POINT('Ctrl Pts',(7.,303.648925943689,-0.0327551936971888));
#9743=CARTESIAN_POINT('Ctrl Pts',(7.00877672769909,303.786425943689,1.84288915332067));
#9744=CARTESIAN_POINT('Ctrl Pts',(6.07855542333967,303.923925943689,3.47163317015236));
#9745=CARTESIAN_POINT('Ctrl Pts',(5.14833411898025,304.061425943689,5.10037718698404));
#9746=CARTESIAN_POINT('Ctrl Pts',(3.52836682984765,304.198925943689,6.04580022964248));
#9747=CARTESIAN_POINT('Ctrl Pts',(1.90839954071505,304.336425943689,6.99122327230091));
#9748=CARTESIAN_POINT('Ctrl Pts',(0.0327551936971892,304.473925943689,7.));
#9749=CARTESIAN_POINT('Ctrl Pts',(-1.84288915332067,304.611425943689,7.00877672769909));
#9750=CARTESIAN_POINT('Ctrl Pts',(-3.47163317015235,304.748925943689,6.07855542333967));
#9751=CARTESIAN_POINT('Ctrl Pts',(-5.10037718698404,304.886425943689,5.14833411898025));
#9752=CARTESIAN_POINT('Ctrl Pts',(-6.04580022964248,305.023925943689,3.52836682984765));
#9753=CARTESIAN_POINT('Ctrl Pts',(-6.99122327230091,305.161425943689,1.90839954071505));
#9754=CARTESIAN_POINT('Ctrl Pts',(-7.,305.298925943689,0.0327551936971879));
#9755=CARTESIAN_POINT('Ctrl Pts',(-7.00877672769909,305.436425943689,-1.84288915332067));
#9756=CARTESIAN_POINT('Ctrl Pts',(-6.07855542333967,305.573925943689,-3.47163317015236));
#9757=CARTESIAN_POINT('Ctrl Pts',(-5.14833411898024,305.711425943689,-5.10037718698404));
#9758=CARTESIAN_POINT('Ctrl Pts',(-3.52836682984765,305.848925943689,-6.04580022964248));
#9759=CARTESIAN_POINT('Ctrl Pts',(-1.90839954071505,305.986425943689,-6.99122327230092));
#9760=CARTESIAN_POINT('Ctrl Pts',(-0.0327551936971884,306.123925943689,
-7.));
#9761=CARTESIAN_POINT('Ctrl Pts',(1.84288915332067,306.261425943689,-7.00877672769909));
#9762=CARTESIAN_POINT('Ctrl Pts',(3.47163317015236,306.398925943689,-6.07855542333967));
#9763=CARTESIAN_POINT('Ctrl Pts',(5.10037718698404,306.536425943689,-5.14833411898024));
#9764=CARTESIAN_POINT('Ctrl Pts',(6.04580022964248,306.673925943689,-3.52836682984765));
#9765=CARTESIAN_POINT('Ctrl Pts',(6.99122327230092,306.811425943689,-1.90839954071505));
#9766=CARTESIAN_POINT('Ctrl Pts',(7.,306.948925943689,-0.0327551936971888));
#9767=CARTESIAN_POINT('Ctrl Pts',(7.00877672769909,307.086425943689,1.84288915332067));
#9768=CARTESIAN_POINT('Ctrl Pts',(6.07855542333967,307.223925943689,3.47163317015236));
#9769=CARTESIAN_POINT('Ctrl Pts',(5.14833411898025,307.361425943689,5.10037718698404));
#9770=CARTESIAN_POINT('Ctrl Pts',(3.52836682984765,307.498925943689,6.04580022964248));
#9771=CARTESIAN_POINT('Ctrl Pts',(1.90839954071505,307.636425943689,6.99122327230091));
#9772=CARTESIAN_POINT('Ctrl Pts',(0.0327551936971892,307.773925943689,7.));
#9773=CARTESIAN_POINT('Ctrl Pts',(-1.84288915332067,307.911425943689,7.00877672769909));
#9774=CARTESIAN_POINT('Ctrl Pts',(-3.47163317015235,308.048925943689,6.07855542333967));
#9775=CARTESIAN_POINT('Ctrl Pts',(-5.10037718698404,308.186425943689,5.14833411898025));
#9776=CARTESIAN_POINT('Ctrl Pts',(-6.04580022964248,308.323925943689,3.52836682984765));
#9777=CARTESIAN_POINT('Ctrl Pts',(-6.99122327230091,308.461425943689,1.90839954071505));
#9778=CARTESIAN_POINT('Ctrl Pts',(-7.,308.598925943689,0.0327551936971879));
#9779=CARTESIAN_POINT('Ctrl Pts',(-7.00877672769909,308.736425943689,-1.84288915332067));
#9780=CARTESIAN_POINT('Ctrl Pts',(-6.07855542333967,308.873925943689,-3.47163317015236));
#9781=CARTESIAN_POINT('Ctrl Pts',(-5.14833411898024,309.011425943689,-5.10037718698404));
#9782=CARTESIAN_POINT('Ctrl Pts',(-3.52836682984765,309.148925943689,-6.04580022964248));
#9783=CARTESIAN_POINT('Ctrl Pts',(-1.90839954071505,309.286425943689,-6.99122327230092));
#9784=CARTESIAN_POINT('Ctrl Pts',(-0.0327551936971884,309.423925943689,
-7.));
#9785=CARTESIAN_POINT('Ctrl Pts',(1.84288915332067,309.561425943689,-7.00877672769909));
#9786=CARTESIAN_POINT('Ctrl Pts',(3.47163317015236,309.698925943689,-6.07855542333967));
#9787=CARTESIAN_POINT('Ctrl Pts',(5.10037718698404,309.836425943689,-5.14833411898024));
#9788=CARTESIAN_POINT('Ctrl Pts',(6.04580022964248,309.973925943689,-3.52836682984765));
#9789=CARTESIAN_POINT('Ctrl Pts',(6.99122327230092,310.111425943689,-1.90839954071505));
#9790=CARTESIAN_POINT('Ctrl Pts',(7.,310.248925943689,-0.0327551936971888));
#9791=CARTESIAN_POINT('Ctrl Pts',(7.00877672769909,310.386425943689,1.84288915332067));
#9792=CARTESIAN_POINT('Ctrl Pts',(6.07855542333967,310.523925943689,3.47163317015236));
#9793=CARTESIAN_POINT('Ctrl Pts',(5.14833411898025,310.661425943689,5.10037718698404));
#9794=CARTESIAN_POINT('Ctrl Pts',(3.52836682984765,310.798925943689,6.04580022964248));
#9795=CARTESIAN_POINT('Ctrl Pts',(1.90839954071505,310.936425943689,6.99122327230091));
#9796=CARTESIAN_POINT('Ctrl Pts',(0.0327551936971892,311.073925943689,7.));
#9797=CARTESIAN_POINT('Ctrl Pts',(-1.84288915332067,311.211425943689,7.00877672769909));
#9798=CARTESIAN_POINT('Ctrl Pts',(-3.47163317015235,311.348925943689,6.07855542333967));
#9799=CARTESIAN_POINT('Ctrl Pts',(-5.10037718698404,311.486425943689,5.14833411898025));
#9800=CARTESIAN_POINT('Ctrl Pts',(-6.04580022964248,311.623925943689,3.52836682984765));
#9801=CARTESIAN_POINT('Ctrl Pts',(-6.99122327230091,311.761425943689,1.90839954071505));
#9802=CARTESIAN_POINT('Ctrl Pts',(-7.,311.898925943689,0.0327551936971879));
#9803=CARTESIAN_POINT('Ctrl Pts',(-7.00877672769909,312.036425943689,-1.84288915332067));
#9804=CARTESIAN_POINT('Ctrl Pts',(-6.07855542333967,312.173925943689,-3.47163317015236));
#9805=CARTESIAN_POINT('Ctrl Pts',(-5.14833411898024,312.311425943689,-5.10037718698404));
#9806=CARTESIAN_POINT('Ctrl Pts',(-3.52836682984765,312.448925943689,-6.04580022964248));
#9807=CARTESIAN_POINT('Ctrl Pts',(-1.90839954071505,312.586425943689,-6.99122327230092));
#9808=CARTESIAN_POINT('Ctrl Pts',(-0.0327551936971884,312.723925943689,
-7.));
#9809=CARTESIAN_POINT('Ctrl Pts',(1.84288915332067,312.861425943689,-7.00877672769909));
#9810=CARTESIAN_POINT('Ctrl Pts',(3.47163317015236,312.998925943689,-6.07855542333967));
#9811=CARTESIAN_POINT('Ctrl Pts',(5.10037718698404,313.136425943689,-5.14833411898024));
#9812=CARTESIAN_POINT('Ctrl Pts',(6.04580022964248,313.273925943689,-3.52836682984765));
#9813=CARTESIAN_POINT('Ctrl Pts',(6.99122327230092,313.411425943689,-1.90839954071505));
#9814=CARTESIAN_POINT('Ctrl Pts',(7.,313.548925943689,-0.0327551936971888));
#9815=CARTESIAN_POINT('Ctrl Pts',(7.00877672769909,313.686425943689,1.84288915332067));
#9816=CARTESIAN_POINT('Ctrl Pts',(6.07855542333967,313.823925943689,3.47163317015236));
#9817=CARTESIAN_POINT('Ctrl Pts',(5.14833411898025,313.961425943689,5.10037718698404));
#9818=CARTESIAN_POINT('Ctrl Pts',(3.52836682984765,314.098925943689,6.04580022964248));
#9819=CARTESIAN_POINT('Ctrl Pts',(1.90839954071505,314.236425943689,6.99122327230091));
#9820=CARTESIAN_POINT('Ctrl Pts',(0.0327551936971892,314.373925943689,7.));
#9821=CARTESIAN_POINT('Ctrl Pts',(-1.84288915332067,314.511425943689,7.00877672769909));
#9822=CARTESIAN_POINT('Ctrl Pts',(-3.47163317015235,314.648925943689,6.07855542333967));
#9823=CARTESIAN_POINT('Ctrl Pts',(-5.10037718698404,314.786425943689,5.14833411898025));
#9824=CARTESIAN_POINT('Ctrl Pts',(-6.04580022964248,314.923925943689,3.52836682984765));
#9825=CARTESIAN_POINT('Ctrl Pts',(-6.99122327230091,315.061425943689,1.90839954071505));
#9826=CARTESIAN_POINT('Ctrl Pts',(-7.,315.198925943689,0.0327551936971879));
#9827=CARTESIAN_POINT('Ctrl Pts',(-7.00877672769909,315.336425943689,-1.84288915332067));
#9828=CARTESIAN_POINT('Ctrl Pts',(-6.07855542333967,315.473925943689,-3.47163317015236));
#9829=CARTESIAN_POINT('Ctrl Pts',(-5.14833411898024,315.611425943689,-5.10037718698404));
#9830=CARTESIAN_POINT('Ctrl Pts',(-3.52836682984765,315.748925943689,-6.04580022964248));
#9831=CARTESIAN_POINT('Ctrl Pts',(-1.90839954071505,315.886425943689,-6.99122327230092));
#9832=CARTESIAN_POINT('Ctrl Pts',(-0.0327551936971884,316.023925943689,
-7.));
#9833=CARTESIAN_POINT('Ctrl Pts',(1.84288915332067,316.161425943689,-7.00877672769909));
#9834=CARTESIAN_POINT('Ctrl Pts',(3.47163317015236,316.298925943689,-6.07855542333967));
#9835=CARTESIAN_POINT('Ctrl Pts',(5.10037718698404,316.436425943689,-5.14833411898024));
#9836=CARTESIAN_POINT('Ctrl Pts',(6.04580022964248,316.573925943689,-3.52836682984765));
#9837=CARTESIAN_POINT('Ctrl Pts',(6.99122327230092,316.711425943689,-1.90839954071505));
#9838=CARTESIAN_POINT('Ctrl Pts',(7.,316.848925943689,-0.0327551936971888));
#9839=CARTESIAN_POINT('Ctrl Pts',(7.00877672769909,316.986425943689,1.84288915332067));
#9840=CARTESIAN_POINT('Ctrl Pts',(6.07855542333967,317.123925943689,3.47163317015236));
#9841=CARTESIAN_POINT('Ctrl Pts',(5.14833411898025,317.261425943689,5.10037718698404));
#9842=CARTESIAN_POINT('Ctrl Pts',(3.52836682984765,317.398925943689,6.04580022964248));
#9843=CARTESIAN_POINT('Ctrl Pts',(1.90839954071505,317.536425943689,6.99122327230091));
#9844=CARTESIAN_POINT('Ctrl Pts',(0.0327551936971892,317.673925943689,7.));
#9845=CARTESIAN_POINT('Ctrl Pts',(-1.84288915332067,317.811425943689,7.00877672769909));
#9846=CARTESIAN_POINT('Ctrl Pts',(-3.47163317015235,317.948925943689,6.07855542333967));
#9847=CARTESIAN_POINT('Ctrl Pts',(-5.10037718698404,318.086425943689,5.14833411898025));
#9848=CARTESIAN_POINT('Ctrl Pts',(-6.04580022964248,318.223925943689,3.52836682984765));
#9849=CARTESIAN_POINT('Ctrl Pts',(-6.99122327230091,318.361425943689,1.90839954071505));
#9850=CARTESIAN_POINT('Ctrl Pts',(-7.,318.498925943689,0.0327551936971879));
#9851=CARTESIAN_POINT('Ctrl Pts',(-7.,284.501074056311,-0.0327551936970413));
#9852=CARTESIAN_POINT('Ctrl Pts',(-6.99122327230096,284.638574056311,-1.9083995407149));
#9853=CARTESIAN_POINT('Ctrl Pts',(-6.04580022964255,284.776074056311,-3.52836682984752));
#9854=CARTESIAN_POINT('Ctrl Pts',(-5.10037718698415,284.913574056311,-5.14833411898014));
#9855=CARTESIAN_POINT('Ctrl Pts',(-3.47163317015249,285.051074056311,-6.07855542333959));
#9856=CARTESIAN_POINT('Ctrl Pts',(-1.84288915332082,285.188574056311,-7.00877672769905));
#9857=CARTESIAN_POINT('Ctrl Pts',(0.0327551936970409,285.326074056311,-7.));
#9858=CARTESIAN_POINT('Ctrl Pts',(1.9083995407149,285.463574056311,-6.99122327230096));
#9859=CARTESIAN_POINT('Ctrl Pts',(3.52836682984752,285.601074056311,-6.04580022964255));
#9860=CARTESIAN_POINT('Ctrl Pts',(5.14833411898014,285.738574056311,-5.10037718698415));
#9861=CARTESIAN_POINT('Ctrl Pts',(6.07855542333959,285.876074056311,-3.47163317015249));
#9862=CARTESIAN_POINT('Ctrl Pts',(7.00877672769905,286.013574056311,-1.84288915332082));
#9863=CARTESIAN_POINT('Ctrl Pts',(7.,286.151074056311,0.0327551936970405));
#9864=CARTESIAN_POINT('Ctrl Pts',(6.99122327230096,286.288574056311,1.9083995407149));
#9865=CARTESIAN_POINT('Ctrl Pts',(6.04580022964255,286.426074056311,3.52836682984752));
#9866=CARTESIAN_POINT('Ctrl Pts',(5.10037718698415,286.563574056311,5.14833411898013));
#9867=CARTESIAN_POINT('Ctrl Pts',(3.47163317015249,286.701074056311,6.07855542333959));
#9868=CARTESIAN_POINT('Ctrl Pts',(1.84288915332082,286.838574056311,7.00877672769905));
#9869=CARTESIAN_POINT('Ctrl Pts',(-0.03275519369704,286.976074056311,7.));
#9870=CARTESIAN_POINT('Ctrl Pts',(-1.9083995407149,287.113574056311,6.99122327230096));
#9871=CARTESIAN_POINT('Ctrl Pts',(-3.52836682984752,287.251074056311,6.04580022964255));
#9872=CARTESIAN_POINT('Ctrl Pts',(-5.14833411898014,287.388574056311,5.10037718698415));
#9873=CARTESIAN_POINT('Ctrl Pts',(-6.07855542333959,287.526074056311,3.47163317015249));
#9874=CARTESIAN_POINT('Ctrl Pts',(-7.00877672769905,287.663574056311,1.84288915332082));
#9875=CARTESIAN_POINT('Ctrl Pts',(-7.,287.801074056311,-0.0327551936970413));
#9876=CARTESIAN_POINT('Ctrl Pts',(-6.99122327230096,287.938574056311,-1.9083995407149));
#9877=CARTESIAN_POINT('Ctrl Pts',(-6.04580022964255,288.076074056311,-3.52836682984752));
#9878=CARTESIAN_POINT('Ctrl Pts',(-5.10037718698415,288.213574056311,-5.14833411898014));
#9879=CARTESIAN_POINT('Ctrl Pts',(-3.47163317015249,288.351074056311,-6.07855542333959));
#9880=CARTESIAN_POINT('Ctrl Pts',(-1.84288915332082,288.488574056311,-7.00877672769905));
#9881=CARTESIAN_POINT('Ctrl Pts',(0.0327551936970409,288.626074056311,-7.));
#9882=CARTESIAN_POINT('Ctrl Pts',(1.9083995407149,288.763574056311,-6.99122327230096));
#9883=CARTESIAN_POINT('Ctrl Pts',(3.52836682984752,288.901074056311,-6.04580022964255));
#9884=CARTESIAN_POINT('Ctrl Pts',(5.14833411898014,289.038574056311,-5.10037718698415));
#9885=CARTESIAN_POINT('Ctrl Pts',(6.07855542333959,289.176074056311,-3.47163317015249));
#9886=CARTESIAN_POINT('Ctrl Pts',(7.00877672769905,289.313574056311,-1.84288915332082));
#9887=CARTESIAN_POINT('Ctrl Pts',(7.,289.451074056311,0.0327551936970405));
#9888=CARTESIAN_POINT('Ctrl Pts',(6.99122327230096,289.588574056311,1.9083995407149));
#9889=CARTESIAN_POINT('Ctrl Pts',(6.04580022964255,289.726074056311,3.52836682984752));
#9890=CARTESIAN_POINT('Ctrl Pts',(5.10037718698415,289.863574056311,5.14833411898013));
#9891=CARTESIAN_POINT('Ctrl Pts',(3.47163317015249,290.001074056311,6.07855542333959));
#9892=CARTESIAN_POINT('Ctrl Pts',(1.84288915332082,290.138574056311,7.00877672769905));
#9893=CARTESIAN_POINT('Ctrl Pts',(-0.03275519369704,290.276074056311,7.));
#9894=CARTESIAN_POINT('Ctrl Pts',(-1.9083995407149,290.413574056311,6.99122327230096));
#9895=CARTESIAN_POINT('Ctrl Pts',(-3.52836682984752,290.551074056311,6.04580022964255));
#9896=CARTESIAN_POINT('Ctrl Pts',(-5.14833411898014,290.688574056311,5.10037718698415));
#9897=CARTESIAN_POINT('Ctrl Pts',(-6.07855542333959,290.826074056311,3.47163317015249));
#9898=CARTESIAN_POINT('Ctrl Pts',(-7.00877672769905,290.963574056311,1.84288915332082));
#9899=CARTESIAN_POINT('Ctrl Pts',(-7.,291.101074056311,-0.0327551936970413));
#9900=CARTESIAN_POINT('Ctrl Pts',(-6.99122327230096,291.238574056311,-1.9083995407149));
#9901=CARTESIAN_POINT('Ctrl Pts',(-6.04580022964255,291.376074056311,-3.52836682984752));
#9902=CARTESIAN_POINT('Ctrl Pts',(-5.10037718698415,291.513574056311,-5.14833411898014));
#9903=CARTESIAN_POINT('Ctrl Pts',(-3.47163317015249,291.651074056311,-6.07855542333959));
#9904=CARTESIAN_POINT('Ctrl Pts',(-1.84288915332082,291.788574056311,-7.00877672769905));
#9905=CARTESIAN_POINT('Ctrl Pts',(0.0327551936970409,291.926074056311,-7.));
#9906=CARTESIAN_POINT('Ctrl Pts',(1.9083995407149,292.063574056311,-6.99122327230096));
#9907=CARTESIAN_POINT('Ctrl Pts',(3.52836682984752,292.201074056311,-6.04580022964255));
#9908=CARTESIAN_POINT('Ctrl Pts',(5.14833411898014,292.338574056311,-5.10037718698415));
#9909=CARTESIAN_POINT('Ctrl Pts',(6.07855542333959,292.476074056311,-3.47163317015249));
#9910=CARTESIAN_POINT('Ctrl Pts',(7.00877672769905,292.613574056311,-1.84288915332082));
#9911=CARTESIAN_POINT('Ctrl Pts',(7.,292.751074056311,0.0327551936970405));
#9912=CARTESIAN_POINT('Ctrl Pts',(6.99122327230096,292.888574056311,1.9083995407149));
#9913=CARTESIAN_POINT('Ctrl Pts',(6.04580022964255,293.026074056311,3.52836682984752));
#9914=CARTESIAN_POINT('Ctrl Pts',(5.10037718698415,293.163574056311,5.14833411898013));
#9915=CARTESIAN_POINT('Ctrl Pts',(3.47163317015249,293.301074056311,6.07855542333959));
#9916=CARTESIAN_POINT('Ctrl Pts',(1.84288915332082,293.438574056311,7.00877672769905));
#9917=CARTESIAN_POINT('Ctrl Pts',(-0.03275519369704,293.576074056311,7.));
#9918=CARTESIAN_POINT('Ctrl Pts',(-1.9083995407149,293.713574056311,6.99122327230096));
#9919=CARTESIAN_POINT('Ctrl Pts',(-3.52836682984752,293.851074056311,6.04580022964255));
#9920=CARTESIAN_POINT('Ctrl Pts',(-5.14833411898014,293.988574056311,5.10037718698415));
#9921=CARTESIAN_POINT('Ctrl Pts',(-6.07855542333959,294.126074056311,3.47163317015249));
#9922=CARTESIAN_POINT('Ctrl Pts',(-7.00877672769905,294.263574056311,1.84288915332082));
#9923=CARTESIAN_POINT('Ctrl Pts',(-7.,294.401074056311,-0.0327551936970413));
#9924=CARTESIAN_POINT('Ctrl Pts',(-6.99122327230096,294.538574056311,-1.9083995407149));
#9925=CARTESIAN_POINT('Ctrl Pts',(-6.04580022964255,294.676074056311,-3.52836682984752));
#9926=CARTESIAN_POINT('Ctrl Pts',(-5.10037718698415,294.813574056311,-5.14833411898014));
#9927=CARTESIAN_POINT('Ctrl Pts',(-3.47163317015249,294.951074056311,-6.07855542333959));
#9928=CARTESIAN_POINT('Ctrl Pts',(-1.84288915332082,295.088574056311,-7.00877672769905));
#9929=CARTESIAN_POINT('Ctrl Pts',(0.0327551936970409,295.226074056311,-7.));
#9930=CARTESIAN_POINT('Ctrl Pts',(1.9083995407149,295.363574056311,-6.99122327230096));
#9931=CARTESIAN_POINT('Ctrl Pts',(3.52836682984752,295.501074056311,-6.04580022964255));
#9932=CARTESIAN_POINT('Ctrl Pts',(5.14833411898014,295.638574056311,-5.10037718698415));
#9933=CARTESIAN_POINT('Ctrl Pts',(6.07855542333959,295.776074056311,-3.47163317015249));
#9934=CARTESIAN_POINT('Ctrl Pts',(7.00877672769905,295.913574056311,-1.84288915332082));
#9935=CARTESIAN_POINT('Ctrl Pts',(7.,296.051074056311,0.0327551936970405));
#9936=CARTESIAN_POINT('Ctrl Pts',(6.99122327230096,296.188574056311,1.9083995407149));
#9937=CARTESIAN_POINT('Ctrl Pts',(6.04580022964255,296.326074056311,3.52836682984752));
#9938=CARTESIAN_POINT('Ctrl Pts',(5.10037718698415,296.463574056311,5.14833411898013));
#9939=CARTESIAN_POINT('Ctrl Pts',(3.47163317015249,296.601074056311,6.07855542333959));
#9940=CARTESIAN_POINT('Ctrl Pts',(1.84288915332082,296.738574056311,7.00877672769905));
#9941=CARTESIAN_POINT('Ctrl Pts',(-0.03275519369704,296.876074056311,7.));
#9942=CARTESIAN_POINT('Ctrl Pts',(-1.9083995407149,297.013574056311,6.99122327230096));
#9943=CARTESIAN_POINT('Ctrl Pts',(-3.52836682984752,297.151074056311,6.04580022964255));
#9944=CARTESIAN_POINT('Ctrl Pts',(-5.14833411898014,297.288574056311,5.10037718698415));
#9945=CARTESIAN_POINT('Ctrl Pts',(-6.07855542333959,297.426074056311,3.47163317015249));
#9946=CARTESIAN_POINT('Ctrl Pts',(-7.00877672769905,297.563574056311,1.84288915332082));
#9947=CARTESIAN_POINT('Ctrl Pts',(-7.,297.701074056311,-0.0327551936970413));
#9948=CARTESIAN_POINT('Ctrl Pts',(-6.99122327230096,297.838574056311,-1.9083995407149));
#9949=CARTESIAN_POINT('Ctrl Pts',(-6.04580022964255,297.976074056311,-3.52836682984752));
#9950=CARTESIAN_POINT('Ctrl Pts',(-5.10037718698415,298.113574056311,-5.14833411898014));
#9951=CARTESIAN_POINT('Ctrl Pts',(-3.47163317015249,298.251074056311,-6.07855542333959));
#9952=CARTESIAN_POINT('Ctrl Pts',(-1.84288915332082,298.388574056311,-7.00877672769905));
#9953=CARTESIAN_POINT('Ctrl Pts',(0.0327551936970409,298.526074056311,-7.));
#9954=CARTESIAN_POINT('Ctrl Pts',(1.9083995407149,298.663574056311,-6.99122327230096));
#9955=CARTESIAN_POINT('Ctrl Pts',(3.52836682984752,298.801074056311,-6.04580022964255));
#9956=CARTESIAN_POINT('Ctrl Pts',(5.14833411898014,298.938574056311,-5.10037718698415));
#9957=CARTESIAN_POINT('Ctrl Pts',(6.07855542333959,299.076074056311,-3.47163317015249));
#9958=CARTESIAN_POINT('Ctrl Pts',(7.00877672769905,299.213574056311,-1.84288915332082));
#9959=CARTESIAN_POINT('Ctrl Pts',(7.,299.351074056311,0.0327551936970405));
#9960=CARTESIAN_POINT('Ctrl Pts',(6.99122327230096,299.488574056311,1.9083995407149));
#9961=CARTESIAN_POINT('Ctrl Pts',(6.04580022964255,299.626074056311,3.52836682984752));
#9962=CARTESIAN_POINT('Ctrl Pts',(5.10037718698415,299.763574056311,5.14833411898013));
#9963=CARTESIAN_POINT('Ctrl Pts',(3.47163317015249,299.901074056311,6.07855542333959));
#9964=CARTESIAN_POINT('Ctrl Pts',(1.84288915332082,300.038574056311,7.00877672769905));
#9965=CARTESIAN_POINT('Ctrl Pts',(-0.03275519369704,300.176074056311,7.));
#9966=CARTESIAN_POINT('Ctrl Pts',(-1.9083995407149,300.313574056311,6.99122327230096));
#9967=CARTESIAN_POINT('Ctrl Pts',(-3.52836682984752,300.451074056311,6.04580022964255));
#9968=CARTESIAN_POINT('Ctrl Pts',(-5.14833411898014,300.588574056311,5.10037718698415));
#9969=CARTESIAN_POINT('Ctrl Pts',(-6.07855542333959,300.726074056311,3.47163317015249));
#9970=CARTESIAN_POINT('Ctrl Pts',(-7.00877672769905,300.863574056311,1.84288915332082));
#9971=CARTESIAN_POINT('Ctrl Pts',(-7.,301.001074056311,-0.0327551936970413));
#9972=CARTESIAN_POINT('Ctrl Pts',(-6.99122327230096,301.138574056311,-1.9083995407149));
#9973=CARTESIAN_POINT('Ctrl Pts',(-6.04580022964255,301.276074056311,-3.52836682984752));
#9974=CARTESIAN_POINT('Ctrl Pts',(-5.10037718698415,301.413574056311,-5.14833411898014));
#9975=CARTESIAN_POINT('Ctrl Pts',(-3.47163317015249,301.551074056311,-6.07855542333959));
#9976=CARTESIAN_POINT('Ctrl Pts',(-1.84288915332082,301.688574056311,-7.00877672769905));
#9977=CARTESIAN_POINT('Ctrl Pts',(0.0327551936970409,301.826074056311,-7.));
#9978=CARTESIAN_POINT('Ctrl Pts',(1.9083995407149,301.963574056311,-6.99122327230096));
#9979=CARTESIAN_POINT('Ctrl Pts',(3.52836682984752,302.101074056311,-6.04580022964255));
#9980=CARTESIAN_POINT('Ctrl Pts',(5.14833411898014,302.238574056311,-5.10037718698415));
#9981=CARTESIAN_POINT('Ctrl Pts',(6.07855542333959,302.376074056311,-3.47163317015249));
#9982=CARTESIAN_POINT('Ctrl Pts',(7.00877672769905,302.513574056311,-1.84288915332082));
#9983=CARTESIAN_POINT('Ctrl Pts',(7.,302.651074056311,0.0327551936970405));
#9984=CARTESIAN_POINT('Ctrl Pts',(6.99122327230096,302.788574056311,1.9083995407149));
#9985=CARTESIAN_POINT('Ctrl Pts',(6.04580022964255,302.926074056311,3.52836682984752));
#9986=CARTESIAN_POINT('Ctrl Pts',(5.10037718698415,303.063574056311,5.14833411898013));
#9987=CARTESIAN_POINT('Ctrl Pts',(3.47163317015249,303.201074056311,6.07855542333959));
#9988=CARTESIAN_POINT('Ctrl Pts',(1.84288915332082,303.338574056311,7.00877672769905));
#9989=CARTESIAN_POINT('Ctrl Pts',(-0.03275519369704,303.476074056311,7.));
#9990=CARTESIAN_POINT('Ctrl Pts',(-1.9083995407149,303.613574056311,6.99122327230096));
#9991=CARTESIAN_POINT('Ctrl Pts',(-3.52836682984752,303.751074056311,6.04580022964255));
#9992=CARTESIAN_POINT('Ctrl Pts',(-5.14833411898014,303.888574056311,5.10037718698415));
#9993=CARTESIAN_POINT('Ctrl Pts',(-6.07855542333959,304.026074056311,3.47163317015249));
#9994=CARTESIAN_POINT('Ctrl Pts',(-7.00877672769905,304.163574056311,1.84288915332082));
#9995=CARTESIAN_POINT('Ctrl Pts',(-7.,304.301074056311,-0.0327551936970413));
#9996=CARTESIAN_POINT('Ctrl Pts',(-6.99122327230096,304.438574056311,-1.9083995407149));
#9997=CARTESIAN_POINT('Ctrl Pts',(-6.04580022964255,304.576074056311,-3.52836682984752));
#9998=CARTESIAN_POINT('Ctrl Pts',(-5.10037718698415,304.713574056311,-5.14833411898014));
#9999=CARTESIAN_POINT('Ctrl Pts',(-3.47163317015249,304.851074056311,-6.07855542333959));
#10000=CARTESIAN_POINT('Ctrl Pts',(-1.84288915332082,304.988574056311,-7.00877672769905));
#10001=CARTESIAN_POINT('Ctrl Pts',(0.0327551936970409,305.126074056311,
-7.));
#10002=CARTESIAN_POINT('Ctrl Pts',(1.9083995407149,305.263574056311,-6.99122327230096));
#10003=CARTESIAN_POINT('Ctrl Pts',(3.52836682984752,305.401074056311,-6.04580022964255));
#10004=CARTESIAN_POINT('Ctrl Pts',(5.14833411898014,305.538574056311,-5.10037718698415));
#10005=CARTESIAN_POINT('Ctrl Pts',(6.07855542333959,305.676074056311,-3.47163317015249));
#10006=CARTESIAN_POINT('Ctrl Pts',(7.00877672769905,305.813574056311,-1.84288915332082));
#10007=CARTESIAN_POINT('Ctrl Pts',(7.,305.951074056311,0.0327551936970405));
#10008=CARTESIAN_POINT('Ctrl Pts',(6.99122327230096,306.088574056311,1.9083995407149));
#10009=CARTESIAN_POINT('Ctrl Pts',(6.04580022964255,306.226074056311,3.52836682984752));
#10010=CARTESIAN_POINT('Ctrl Pts',(5.10037718698415,306.363574056311,5.14833411898013));
#10011=CARTESIAN_POINT('Ctrl Pts',(3.47163317015249,306.501074056311,6.07855542333959));
#10012=CARTESIAN_POINT('Ctrl Pts',(1.84288915332082,306.638574056311,7.00877672769905));
#10013=CARTESIAN_POINT('Ctrl Pts',(-0.03275519369704,306.776074056311,7.));
#10014=CARTESIAN_POINT('Ctrl Pts',(-1.9083995407149,306.913574056311,6.99122327230096));
#10015=CARTESIAN_POINT('Ctrl Pts',(-3.52836682984752,307.051074056311,6.04580022964255));
#10016=CARTESIAN_POINT('Ctrl Pts',(-5.14833411898014,307.188574056311,5.10037718698415));
#10017=CARTESIAN_POINT('Ctrl Pts',(-6.07855542333959,307.326074056311,3.47163317015249));
#10018=CARTESIAN_POINT('Ctrl Pts',(-7.00877672769905,307.463574056311,1.84288915332082));
#10019=CARTESIAN_POINT('Ctrl Pts',(-7.,307.601074056311,-0.0327551936970413));
#10020=CARTESIAN_POINT('Ctrl Pts',(-6.99122327230096,307.738574056311,-1.9083995407149));
#10021=CARTESIAN_POINT('Ctrl Pts',(-6.04580022964255,307.876074056311,-3.52836682984752));
#10022=CARTESIAN_POINT('Ctrl Pts',(-5.10037718698415,308.013574056311,-5.14833411898014));
#10023=CARTESIAN_POINT('Ctrl Pts',(-3.47163317015249,308.151074056311,-6.07855542333959));
#10024=CARTESIAN_POINT('Ctrl Pts',(-1.84288915332082,308.288574056311,-7.00877672769905));
#10025=CARTESIAN_POINT('Ctrl Pts',(0.0327551936970409,308.426074056311,
-7.));
#10026=CARTESIAN_POINT('Ctrl Pts',(1.9083995407149,308.563574056311,-6.99122327230096));
#10027=CARTESIAN_POINT('Ctrl Pts',(3.52836682984752,308.701074056311,-6.04580022964255));
#10028=CARTESIAN_POINT('Ctrl Pts',(5.14833411898014,308.838574056311,-5.10037718698415));
#10029=CARTESIAN_POINT('Ctrl Pts',(6.07855542333959,308.976074056311,-3.47163317015249));
#10030=CARTESIAN_POINT('Ctrl Pts',(7.00877672769905,309.113574056311,-1.84288915332082));
#10031=CARTESIAN_POINT('Ctrl Pts',(7.,309.251074056311,0.0327551936970405));
#10032=CARTESIAN_POINT('Ctrl Pts',(6.99122327230096,309.388574056311,1.9083995407149));
#10033=CARTESIAN_POINT('Ctrl Pts',(6.04580022964255,309.526074056311,3.52836682984752));
#10034=CARTESIAN_POINT('Ctrl Pts',(5.10037718698415,309.663574056311,5.14833411898013));
#10035=CARTESIAN_POINT('Ctrl Pts',(3.47163317015249,309.801074056311,6.07855542333959));
#10036=CARTESIAN_POINT('Ctrl Pts',(1.84288915332082,309.938574056311,7.00877672769905));
#10037=CARTESIAN_POINT('Ctrl Pts',(-0.03275519369704,310.076074056311,7.));
#10038=CARTESIAN_POINT('Ctrl Pts',(-1.9083995407149,310.213574056311,6.99122327230096));
#10039=CARTESIAN_POINT('Ctrl Pts',(-3.52836682984752,310.351074056311,6.04580022964255));
#10040=CARTESIAN_POINT('Ctrl Pts',(-5.14833411898014,310.488574056311,5.10037718698415));
#10041=CARTESIAN_POINT('Ctrl Pts',(-6.07855542333959,310.626074056311,3.47163317015249));
#10042=CARTESIAN_POINT('Ctrl Pts',(-7.00877672769905,310.763574056311,1.84288915332082));
#10043=CARTESIAN_POINT('Ctrl Pts',(-7.,310.901074056311,-0.0327551936970413));
#10044=CARTESIAN_POINT('Ctrl Pts',(-6.99122327230096,311.038574056311,-1.9083995407149));
#10045=CARTESIAN_POINT('Ctrl Pts',(-6.04580022964255,311.176074056311,-3.52836682984752));
#10046=CARTESIAN_POINT('Ctrl Pts',(-5.10037718698415,311.313574056311,-5.14833411898014));
#10047=CARTESIAN_POINT('Ctrl Pts',(-3.47163317015249,311.451074056311,-6.07855542333959));
#10048=CARTESIAN_POINT('Ctrl Pts',(-1.84288915332082,311.588574056311,-7.00877672769905));
#10049=CARTESIAN_POINT('Ctrl Pts',(0.0327551936970409,311.726074056311,
-7.));
#10050=CARTESIAN_POINT('Ctrl Pts',(1.9083995407149,311.863574056311,-6.99122327230096));
#10051=CARTESIAN_POINT('Ctrl Pts',(3.52836682984752,312.001074056311,-6.04580022964255));
#10052=CARTESIAN_POINT('Ctrl Pts',(5.14833411898014,312.138574056311,-5.10037718698415));
#10053=CARTESIAN_POINT('Ctrl Pts',(6.07855542333959,312.276074056311,-3.47163317015249));
#10054=CARTESIAN_POINT('Ctrl Pts',(7.00877672769905,312.413574056311,-1.84288915332082));
#10055=CARTESIAN_POINT('Ctrl Pts',(7.,312.551074056311,0.0327551936970405));
#10056=CARTESIAN_POINT('Ctrl Pts',(6.99122327230096,312.688574056311,1.9083995407149));
#10057=CARTESIAN_POINT('Ctrl Pts',(6.04580022964255,312.826074056311,3.52836682984752));
#10058=CARTESIAN_POINT('Ctrl Pts',(5.10037718698415,312.963574056311,5.14833411898013));
#10059=CARTESIAN_POINT('Ctrl Pts',(3.47163317015249,313.101074056311,6.07855542333959));
#10060=CARTESIAN_POINT('Ctrl Pts',(1.84288915332082,313.238574056311,7.00877672769905));
#10061=CARTESIAN_POINT('Ctrl Pts',(-0.03275519369704,313.376074056311,7.));
#10062=CARTESIAN_POINT('Ctrl Pts',(-1.9083995407149,313.513574056311,6.99122327230096));
#10063=CARTESIAN_POINT('Ctrl Pts',(-3.52836682984752,313.651074056311,6.04580022964255));
#10064=CARTESIAN_POINT('Ctrl Pts',(-5.14833411898014,313.788574056311,5.10037718698415));
#10065=CARTESIAN_POINT('Ctrl Pts',(-6.07855542333959,313.926074056311,3.47163317015249));
#10066=CARTESIAN_POINT('Ctrl Pts',(-7.00877672769905,314.063574056311,1.84288915332082));
#10067=CARTESIAN_POINT('Ctrl Pts',(-7.,314.201074056311,-0.0327551936970413));
#10068=CARTESIAN_POINT('Ctrl Pts',(-6.99122327230096,314.338574056311,-1.9083995407149));
#10069=CARTESIAN_POINT('Ctrl Pts',(-6.04580022964255,314.476074056311,-3.52836682984752));
#10070=CARTESIAN_POINT('Ctrl Pts',(-5.10037718698415,314.613574056311,-5.14833411898014));
#10071=CARTESIAN_POINT('Ctrl Pts',(-3.47163317015249,314.751074056311,-6.07855542333959));
#10072=CARTESIAN_POINT('Ctrl Pts',(-1.84288915332082,314.888574056311,-7.00877672769905));
#10073=CARTESIAN_POINT('Ctrl Pts',(0.0327551936970409,315.026074056311,
-7.));
#10074=CARTESIAN_POINT('Ctrl Pts',(1.9083995407149,315.163574056311,-6.99122327230096));
#10075=CARTESIAN_POINT('Ctrl Pts',(3.52836682984752,315.301074056311,-6.04580022964255));
#10076=CARTESIAN_POINT('Ctrl Pts',(5.14833411898014,315.438574056311,-5.10037718698415));
#10077=CARTESIAN_POINT('Ctrl Pts',(6.07855542333959,315.576074056311,-3.47163317015249));
#10078=CARTESIAN_POINT('Ctrl Pts',(7.00877672769905,315.713574056311,-1.84288915332082));
#10079=CARTESIAN_POINT('Ctrl Pts',(7.,315.851074056311,0.0327551936970405));
#10080=CARTESIAN_POINT('Ctrl Pts',(6.99122327230096,315.988574056311,1.9083995407149));
#10081=CARTESIAN_POINT('Ctrl Pts',(6.04580022964255,316.126074056311,3.52836682984752));
#10082=CARTESIAN_POINT('Ctrl Pts',(5.10037718698415,316.263574056311,5.14833411898013));
#10083=CARTESIAN_POINT('Ctrl Pts',(3.47163317015249,316.401074056311,6.07855542333959));
#10084=CARTESIAN_POINT('Ctrl Pts',(1.84288915332082,316.538574056311,7.00877672769905));
#10085=CARTESIAN_POINT('Ctrl Pts',(-0.03275519369704,316.676074056311,7.));
#10086=CARTESIAN_POINT('Ctrl Pts',(-1.9083995407149,316.813574056311,6.99122327230096));
#10087=CARTESIAN_POINT('Ctrl Pts',(-3.52836682984752,316.951074056311,6.04580022964255));
#10088=CARTESIAN_POINT('Ctrl Pts',(-5.14833411898014,317.088574056311,5.10037718698415));
#10089=CARTESIAN_POINT('Ctrl Pts',(-6.07855542333959,317.226074056311,3.47163317015249));
#10090=CARTESIAN_POINT('Ctrl Pts',(-7.00877672769905,317.363574056311,1.84288915332082));
#10091=CARTESIAN_POINT('Ctrl Pts',(-7.,317.501074056311,-0.0327551936970413));
#10092=CARTESIAN_POINT('Ctrl Pts',(-8.,284.501074056311,-0.0327551936970314));
#10093=CARTESIAN_POINT('Ctrl Pts',(-7.99122327230096,284.638574056311,-2.17634873314601));
#10094=CARTESIAN_POINT('Ctrl Pts',(-6.911825633427,284.776074056311,-4.02836682984751));
#10095=CARTESIAN_POINT('Ctrl Pts',(-5.83242799455303,284.913574056311,-5.88038492654901));
#10096=CARTESIAN_POINT('Ctrl Pts',(-3.97163317015249,285.051074056311,-6.94458082712403));
#10097=CARTESIAN_POINT('Ctrl Pts',(-2.11083834575195,285.188574056311,-8.00877672769905));
#10098=CARTESIAN_POINT('Ctrl Pts',(0.0327551936970309,285.326074056311,
-8.));
#10099=CARTESIAN_POINT('Ctrl Pts',(2.17634873314601,285.463574056311,-7.99122327230096));
#10100=CARTESIAN_POINT('Ctrl Pts',(4.02836682984751,285.601074056311,-6.911825633427));
#10101=CARTESIAN_POINT('Ctrl Pts',(5.88038492654901,285.738574056311,-5.83242799455303));
#10102=CARTESIAN_POINT('Ctrl Pts',(6.94458082712403,285.876074056311,-3.9716331701525));
#10103=CARTESIAN_POINT('Ctrl Pts',(8.00877672769905,286.013574056311,-2.11083834575195));
#10104=CARTESIAN_POINT('Ctrl Pts',(8.,286.151074056311,0.0327551936970304));
#10105=CARTESIAN_POINT('Ctrl Pts',(7.99122327230096,286.288574056311,2.17634873314601));
#10106=CARTESIAN_POINT('Ctrl Pts',(6.911825633427,286.426074056311,4.02836682984751));
#10107=CARTESIAN_POINT('Ctrl Pts',(5.83242799455304,286.563574056311,5.880384926549));
#10108=CARTESIAN_POINT('Ctrl Pts',(3.9716331701525,286.701074056311,6.94458082712403));
#10109=CARTESIAN_POINT('Ctrl Pts',(2.11083834575196,286.838574056311,8.00877672769905));
#10110=CARTESIAN_POINT('Ctrl Pts',(-0.0327551936970299,286.976074056311,
8.));
#10111=CARTESIAN_POINT('Ctrl Pts',(-2.17634873314601,287.113574056311,7.99122327230096));
#10112=CARTESIAN_POINT('Ctrl Pts',(-4.02836682984751,287.251074056311,6.911825633427));
#10113=CARTESIAN_POINT('Ctrl Pts',(-5.88038492654901,287.388574056311,5.83242799455303));
#10114=CARTESIAN_POINT('Ctrl Pts',(-6.94458082712403,287.526074056311,3.9716331701525));
#10115=CARTESIAN_POINT('Ctrl Pts',(-8.00877672769905,287.663574056311,2.11083834575196));
#10116=CARTESIAN_POINT('Ctrl Pts',(-8.,287.801074056311,-0.0327551936970314));
#10117=CARTESIAN_POINT('Ctrl Pts',(-7.99122327230096,287.938574056311,-2.17634873314601));
#10118=CARTESIAN_POINT('Ctrl Pts',(-6.911825633427,288.076074056311,-4.02836682984751));
#10119=CARTESIAN_POINT('Ctrl Pts',(-5.83242799455303,288.213574056311,-5.88038492654901));
#10120=CARTESIAN_POINT('Ctrl Pts',(-3.97163317015249,288.351074056311,-6.94458082712403));
#10121=CARTESIAN_POINT('Ctrl Pts',(-2.11083834575195,288.488574056311,-8.00877672769905));
#10122=CARTESIAN_POINT('Ctrl Pts',(0.0327551936970309,288.626074056311,
-8.));
#10123=CARTESIAN_POINT('Ctrl Pts',(2.17634873314601,288.763574056311,-7.99122327230096));
#10124=CARTESIAN_POINT('Ctrl Pts',(4.02836682984751,288.901074056311,-6.911825633427));
#10125=CARTESIAN_POINT('Ctrl Pts',(5.88038492654901,289.038574056311,-5.83242799455303));
#10126=CARTESIAN_POINT('Ctrl Pts',(6.94458082712403,289.176074056311,-3.9716331701525));
#10127=CARTESIAN_POINT('Ctrl Pts',(8.00877672769905,289.313574056311,-2.11083834575195));
#10128=CARTESIAN_POINT('Ctrl Pts',(8.,289.451074056311,0.0327551936970304));
#10129=CARTESIAN_POINT('Ctrl Pts',(7.99122327230096,289.588574056311,2.17634873314601));
#10130=CARTESIAN_POINT('Ctrl Pts',(6.911825633427,289.726074056311,4.02836682984751));
#10131=CARTESIAN_POINT('Ctrl Pts',(5.83242799455304,289.863574056311,5.880384926549));
#10132=CARTESIAN_POINT('Ctrl Pts',(3.9716331701525,290.001074056311,6.94458082712403));
#10133=CARTESIAN_POINT('Ctrl Pts',(2.11083834575196,290.138574056311,8.00877672769905));
#10134=CARTESIAN_POINT('Ctrl Pts',(-0.0327551936970299,290.276074056311,
8.));
#10135=CARTESIAN_POINT('Ctrl Pts',(-2.17634873314601,290.413574056311,7.99122327230096));
#10136=CARTESIAN_POINT('Ctrl Pts',(-4.02836682984751,290.551074056311,6.911825633427));
#10137=CARTESIAN_POINT('Ctrl Pts',(-5.88038492654901,290.688574056311,5.83242799455303));
#10138=CARTESIAN_POINT('Ctrl Pts',(-6.94458082712403,290.826074056311,3.9716331701525));
#10139=CARTESIAN_POINT('Ctrl Pts',(-8.00877672769905,290.963574056311,2.11083834575196));
#10140=CARTESIAN_POINT('Ctrl Pts',(-8.,291.101074056311,-0.0327551936970314));
#10141=CARTESIAN_POINT('Ctrl Pts',(-7.99122327230096,291.238574056311,-2.17634873314601));
#10142=CARTESIAN_POINT('Ctrl Pts',(-6.911825633427,291.376074056311,-4.02836682984751));
#10143=CARTESIAN_POINT('Ctrl Pts',(-5.83242799455303,291.513574056311,-5.88038492654901));
#10144=CARTESIAN_POINT('Ctrl Pts',(-3.97163317015249,291.651074056311,-6.94458082712403));
#10145=CARTESIAN_POINT('Ctrl Pts',(-2.11083834575195,291.788574056311,-8.00877672769905));
#10146=CARTESIAN_POINT('Ctrl Pts',(0.0327551936970309,291.926074056311,
-8.));
#10147=CARTESIAN_POINT('Ctrl Pts',(2.17634873314601,292.063574056311,-7.99122327230096));
#10148=CARTESIAN_POINT('Ctrl Pts',(4.02836682984751,292.201074056311,-6.911825633427));
#10149=CARTESIAN_POINT('Ctrl Pts',(5.88038492654901,292.338574056311,-5.83242799455303));
#10150=CARTESIAN_POINT('Ctrl Pts',(6.94458082712403,292.476074056311,-3.9716331701525));
#10151=CARTESIAN_POINT('Ctrl Pts',(8.00877672769905,292.613574056311,-2.11083834575195));
#10152=CARTESIAN_POINT('Ctrl Pts',(8.,292.751074056311,0.0327551936970304));
#10153=CARTESIAN_POINT('Ctrl Pts',(7.99122327230096,292.888574056311,2.17634873314601));
#10154=CARTESIAN_POINT('Ctrl Pts',(6.911825633427,293.026074056311,4.02836682984751));
#10155=CARTESIAN_POINT('Ctrl Pts',(5.83242799455304,293.163574056311,5.880384926549));
#10156=CARTESIAN_POINT('Ctrl Pts',(3.9716331701525,293.301074056311,6.94458082712403));
#10157=CARTESIAN_POINT('Ctrl Pts',(2.11083834575196,293.438574056311,8.00877672769905));
#10158=CARTESIAN_POINT('Ctrl Pts',(-0.0327551936970299,293.576074056311,
8.));
#10159=CARTESIAN_POINT('Ctrl Pts',(-2.17634873314601,293.713574056311,7.99122327230096));
#10160=CARTESIAN_POINT('Ctrl Pts',(-4.02836682984751,293.851074056311,6.911825633427));
#10161=CARTESIAN_POINT('Ctrl Pts',(-5.88038492654901,293.988574056311,5.83242799455303));
#10162=CARTESIAN_POINT('Ctrl Pts',(-6.94458082712403,294.126074056311,3.9716331701525));
#10163=CARTESIAN_POINT('Ctrl Pts',(-8.00877672769905,294.263574056311,2.11083834575196));
#10164=CARTESIAN_POINT('Ctrl Pts',(-8.,294.401074056311,-0.0327551936970314));
#10165=CARTESIAN_POINT('Ctrl Pts',(-7.99122327230096,294.538574056311,-2.17634873314601));
#10166=CARTESIAN_POINT('Ctrl Pts',(-6.911825633427,294.676074056311,-4.02836682984751));
#10167=CARTESIAN_POINT('Ctrl Pts',(-5.83242799455303,294.813574056311,-5.88038492654901));
#10168=CARTESIAN_POINT('Ctrl Pts',(-3.97163317015249,294.951074056311,-6.94458082712403));
#10169=CARTESIAN_POINT('Ctrl Pts',(-2.11083834575195,295.088574056311,-8.00877672769905));
#10170=CARTESIAN_POINT('Ctrl Pts',(0.0327551936970309,295.226074056311,
-8.));
#10171=CARTESIAN_POINT('Ctrl Pts',(2.17634873314601,295.363574056311,-7.99122327230096));
#10172=CARTESIAN_POINT('Ctrl Pts',(4.02836682984751,295.501074056311,-6.911825633427));
#10173=CARTESIAN_POINT('Ctrl Pts',(5.88038492654901,295.638574056311,-5.83242799455303));
#10174=CARTESIAN_POINT('Ctrl Pts',(6.94458082712403,295.776074056311,-3.9716331701525));
#10175=CARTESIAN_POINT('Ctrl Pts',(8.00877672769905,295.913574056311,-2.11083834575195));
#10176=CARTESIAN_POINT('Ctrl Pts',(8.,296.051074056311,0.0327551936970304));
#10177=CARTESIAN_POINT('Ctrl Pts',(7.99122327230096,296.188574056311,2.17634873314601));
#10178=CARTESIAN_POINT('Ctrl Pts',(6.911825633427,296.326074056311,4.02836682984751));
#10179=CARTESIAN_POINT('Ctrl Pts',(5.83242799455304,296.463574056311,5.880384926549));
#10180=CARTESIAN_POINT('Ctrl Pts',(3.9716331701525,296.601074056311,6.94458082712403));
#10181=CARTESIAN_POINT('Ctrl Pts',(2.11083834575196,296.738574056311,8.00877672769905));
#10182=CARTESIAN_POINT('Ctrl Pts',(-0.0327551936970299,296.876074056311,
8.));
#10183=CARTESIAN_POINT('Ctrl Pts',(-2.17634873314601,297.013574056311,7.99122327230096));
#10184=CARTESIAN_POINT('Ctrl Pts',(-4.02836682984751,297.151074056311,6.911825633427));
#10185=CARTESIAN_POINT('Ctrl Pts',(-5.88038492654901,297.288574056311,5.83242799455303));
#10186=CARTESIAN_POINT('Ctrl Pts',(-6.94458082712403,297.426074056311,3.9716331701525));
#10187=CARTESIAN_POINT('Ctrl Pts',(-8.00877672769905,297.563574056311,2.11083834575196));
#10188=CARTESIAN_POINT('Ctrl Pts',(-8.,297.701074056311,-0.0327551936970314));
#10189=CARTESIAN_POINT('Ctrl Pts',(-7.99122327230096,297.838574056311,-2.17634873314601));
#10190=CARTESIAN_POINT('Ctrl Pts',(-6.911825633427,297.976074056311,-4.02836682984751));
#10191=CARTESIAN_POINT('Ctrl Pts',(-5.83242799455303,298.113574056311,-5.88038492654901));
#10192=CARTESIAN_POINT('Ctrl Pts',(-3.97163317015249,298.251074056311,-6.94458082712403));
#10193=CARTESIAN_POINT('Ctrl Pts',(-2.11083834575195,298.388574056311,-8.00877672769905));
#10194=CARTESIAN_POINT('Ctrl Pts',(0.0327551936970309,298.526074056311,
-8.));
#10195=CARTESIAN_POINT('Ctrl Pts',(2.17634873314601,298.663574056311,-7.99122327230096));
#10196=CARTESIAN_POINT('Ctrl Pts',(4.02836682984751,298.801074056311,-6.911825633427));
#10197=CARTESIAN_POINT('Ctrl Pts',(5.88038492654901,298.938574056311,-5.83242799455303));
#10198=CARTESIAN_POINT('Ctrl Pts',(6.94458082712403,299.076074056311,-3.9716331701525));
#10199=CARTESIAN_POINT('Ctrl Pts',(8.00877672769905,299.213574056311,-2.11083834575195));
#10200=CARTESIAN_POINT('Ctrl Pts',(8.,299.351074056311,0.0327551936970304));
#10201=CARTESIAN_POINT('Ctrl Pts',(7.99122327230096,299.488574056311,2.17634873314601));
#10202=CARTESIAN_POINT('Ctrl Pts',(6.911825633427,299.626074056311,4.02836682984751));
#10203=CARTESIAN_POINT('Ctrl Pts',(5.83242799455304,299.763574056311,5.880384926549));
#10204=CARTESIAN_POINT('Ctrl Pts',(3.9716331701525,299.901074056311,6.94458082712403));
#10205=CARTESIAN_POINT('Ctrl Pts',(2.11083834575196,300.038574056311,8.00877672769905));
#10206=CARTESIAN_POINT('Ctrl Pts',(-0.0327551936970299,300.176074056311,
8.));
#10207=CARTESIAN_POINT('Ctrl Pts',(-2.17634873314601,300.313574056311,7.99122327230096));
#10208=CARTESIAN_POINT('Ctrl Pts',(-4.02836682984751,300.451074056311,6.911825633427));
#10209=CARTESIAN_POINT('Ctrl Pts',(-5.88038492654901,300.588574056311,5.83242799455303));
#10210=CARTESIAN_POINT('Ctrl Pts',(-6.94458082712403,300.726074056311,3.9716331701525));
#10211=CARTESIAN_POINT('Ctrl Pts',(-8.00877672769905,300.863574056311,2.11083834575196));
#10212=CARTESIAN_POINT('Ctrl Pts',(-8.,301.001074056311,-0.0327551936970314));
#10213=CARTESIAN_POINT('Ctrl Pts',(-7.99122327230096,301.138574056311,-2.17634873314601));
#10214=CARTESIAN_POINT('Ctrl Pts',(-6.911825633427,301.276074056311,-4.02836682984751));
#10215=CARTESIAN_POINT('Ctrl Pts',(-5.83242799455303,301.413574056311,-5.88038492654901));
#10216=CARTESIAN_POINT('Ctrl Pts',(-3.97163317015249,301.551074056311,-6.94458082712403));
#10217=CARTESIAN_POINT('Ctrl Pts',(-2.11083834575195,301.688574056311,-8.00877672769905));
#10218=CARTESIAN_POINT('Ctrl Pts',(0.0327551936970309,301.826074056311,
-8.));
#10219=CARTESIAN_POINT('Ctrl Pts',(2.17634873314601,301.963574056311,-7.99122327230096));
#10220=CARTESIAN_POINT('Ctrl Pts',(4.02836682984751,302.101074056311,-6.911825633427));
#10221=CARTESIAN_POINT('Ctrl Pts',(5.88038492654901,302.238574056311,-5.83242799455303));
#10222=CARTESIAN_POINT('Ctrl Pts',(6.94458082712403,302.376074056311,-3.9716331701525));
#10223=CARTESIAN_POINT('Ctrl Pts',(8.00877672769905,302.513574056311,-2.11083834575195));
#10224=CARTESIAN_POINT('Ctrl Pts',(8.,302.651074056311,0.0327551936970304));
#10225=CARTESIAN_POINT('Ctrl Pts',(7.99122327230096,302.788574056311,2.17634873314601));
#10226=CARTESIAN_POINT('Ctrl Pts',(6.911825633427,302.926074056311,4.02836682984751));
#10227=CARTESIAN_POINT('Ctrl Pts',(5.83242799455304,303.063574056311,5.880384926549));
#10228=CARTESIAN_POINT('Ctrl Pts',(3.9716331701525,303.201074056311,6.94458082712403));
#10229=CARTESIAN_POINT('Ctrl Pts',(2.11083834575196,303.338574056311,8.00877672769905));
#10230=CARTESIAN_POINT('Ctrl Pts',(-0.0327551936970299,303.476074056311,
8.));
#10231=CARTESIAN_POINT('Ctrl Pts',(-2.17634873314601,303.613574056311,7.99122327230096));
#10232=CARTESIAN_POINT('Ctrl Pts',(-4.02836682984751,303.751074056311,6.911825633427));
#10233=CARTESIAN_POINT('Ctrl Pts',(-5.88038492654901,303.888574056311,5.83242799455303));
#10234=CARTESIAN_POINT('Ctrl Pts',(-6.94458082712403,304.026074056311,3.9716331701525));
#10235=CARTESIAN_POINT('Ctrl Pts',(-8.00877672769905,304.163574056311,2.11083834575196));
#10236=CARTESIAN_POINT('Ctrl Pts',(-8.,304.301074056311,-0.0327551936970314));
#10237=CARTESIAN_POINT('Ctrl Pts',(-7.99122327230096,304.438574056311,-2.17634873314601));
#10238=CARTESIAN_POINT('Ctrl Pts',(-6.911825633427,304.576074056311,-4.02836682984751));
#10239=CARTESIAN_POINT('Ctrl Pts',(-5.83242799455303,304.713574056311,-5.88038492654901));
#10240=CARTESIAN_POINT('Ctrl Pts',(-3.97163317015249,304.851074056311,-6.94458082712403));
#10241=CARTESIAN_POINT('Ctrl Pts',(-2.11083834575195,304.988574056311,-8.00877672769905));
#10242=CARTESIAN_POINT('Ctrl Pts',(0.0327551936970309,305.126074056311,
-8.));
#10243=CARTESIAN_POINT('Ctrl Pts',(2.17634873314601,305.263574056311,-7.99122327230096));
#10244=CARTESIAN_POINT('Ctrl Pts',(4.02836682984751,305.401074056311,-6.911825633427));
#10245=CARTESIAN_POINT('Ctrl Pts',(5.88038492654901,305.538574056311,-5.83242799455303));
#10246=CARTESIAN_POINT('Ctrl Pts',(6.94458082712403,305.676074056311,-3.9716331701525));
#10247=CARTESIAN_POINT('Ctrl Pts',(8.00877672769905,305.813574056311,-2.11083834575195));
#10248=CARTESIAN_POINT('Ctrl Pts',(8.,305.951074056311,0.0327551936970304));
#10249=CARTESIAN_POINT('Ctrl Pts',(7.99122327230096,306.088574056311,2.17634873314601));
#10250=CARTESIAN_POINT('Ctrl Pts',(6.911825633427,306.226074056311,4.02836682984751));
#10251=CARTESIAN_POINT('Ctrl Pts',(5.83242799455304,306.363574056311,5.880384926549));
#10252=CARTESIAN_POINT('Ctrl Pts',(3.9716331701525,306.501074056311,6.94458082712403));
#10253=CARTESIAN_POINT('Ctrl Pts',(2.11083834575196,306.638574056311,8.00877672769905));
#10254=CARTESIAN_POINT('Ctrl Pts',(-0.0327551936970299,306.776074056311,
8.));
#10255=CARTESIAN_POINT('Ctrl Pts',(-2.17634873314601,306.913574056311,7.99122327230096));
#10256=CARTESIAN_POINT('Ctrl Pts',(-4.02836682984751,307.051074056311,6.911825633427));
#10257=CARTESIAN_POINT('Ctrl Pts',(-5.88038492654901,307.188574056311,5.83242799455303));
#10258=CARTESIAN_POINT('Ctrl Pts',(-6.94458082712403,307.326074056311,3.9716331701525));
#10259=CARTESIAN_POINT('Ctrl Pts',(-8.00877672769905,307.463574056311,2.11083834575196));
#10260=CARTESIAN_POINT('Ctrl Pts',(-8.,307.601074056311,-0.0327551936970314));
#10261=CARTESIAN_POINT('Ctrl Pts',(-7.99122327230096,307.738574056311,-2.17634873314601));
#10262=CARTESIAN_POINT('Ctrl Pts',(-6.911825633427,307.876074056311,-4.02836682984751));
#10263=CARTESIAN_POINT('Ctrl Pts',(-5.83242799455303,308.013574056311,-5.88038492654901));
#10264=CARTESIAN_POINT('Ctrl Pts',(-3.97163317015249,308.151074056311,-6.94458082712403));
#10265=CARTESIAN_POINT('Ctrl Pts',(-2.11083834575195,308.288574056311,-8.00877672769905));
#10266=CARTESIAN_POINT('Ctrl Pts',(0.0327551936970309,308.426074056311,
-8.));
#10267=CARTESIAN_POINT('Ctrl Pts',(2.17634873314601,308.563574056311,-7.99122327230096));
#10268=CARTESIAN_POINT('Ctrl Pts',(4.02836682984751,308.701074056311,-6.911825633427));
#10269=CARTESIAN_POINT('Ctrl Pts',(5.88038492654901,308.838574056311,-5.83242799455303));
#10270=CARTESIAN_POINT('Ctrl Pts',(6.94458082712403,308.976074056311,-3.9716331701525));
#10271=CARTESIAN_POINT('Ctrl Pts',(8.00877672769905,309.113574056311,-2.11083834575195));
#10272=CARTESIAN_POINT('Ctrl Pts',(8.,309.251074056311,0.0327551936970304));
#10273=CARTESIAN_POINT('Ctrl Pts',(7.99122327230096,309.388574056311,2.17634873314601));
#10274=CARTESIAN_POINT('Ctrl Pts',(6.911825633427,309.526074056311,4.02836682984751));
#10275=CARTESIAN_POINT('Ctrl Pts',(5.83242799455304,309.663574056311,5.880384926549));
#10276=CARTESIAN_POINT('Ctrl Pts',(3.9716331701525,309.801074056311,6.94458082712403));
#10277=CARTESIAN_POINT('Ctrl Pts',(2.11083834575196,309.938574056311,8.00877672769905));
#10278=CARTESIAN_POINT('Ctrl Pts',(-0.0327551936970299,310.076074056311,
8.));
#10279=CARTESIAN_POINT('Ctrl Pts',(-2.17634873314601,310.213574056311,7.99122327230096));
#10280=CARTESIAN_POINT('Ctrl Pts',(-4.02836682984751,310.351074056311,6.911825633427));
#10281=CARTESIAN_POINT('Ctrl Pts',(-5.88038492654901,310.488574056311,5.83242799455303));
#10282=CARTESIAN_POINT('Ctrl Pts',(-6.94458082712403,310.626074056311,3.9716331701525));
#10283=CARTESIAN_POINT('Ctrl Pts',(-8.00877672769905,310.763574056311,2.11083834575196));
#10284=CARTESIAN_POINT('Ctrl Pts',(-8.,310.901074056311,-0.0327551936970314));
#10285=CARTESIAN_POINT('Ctrl Pts',(-7.99122327230096,311.038574056311,-2.17634873314601));
#10286=CARTESIAN_POINT('Ctrl Pts',(-6.911825633427,311.176074056311,-4.02836682984751));
#10287=CARTESIAN_POINT('Ctrl Pts',(-5.83242799455303,311.313574056311,-5.88038492654901));
#10288=CARTESIAN_POINT('Ctrl Pts',(-3.97163317015249,311.451074056311,-6.94458082712403));
#10289=CARTESIAN_POINT('Ctrl Pts',(-2.11083834575195,311.588574056311,-8.00877672769905));
#10290=CARTESIAN_POINT('Ctrl Pts',(0.0327551936970309,311.726074056311,
-8.));
#10291=CARTESIAN_POINT('Ctrl Pts',(2.17634873314601,311.863574056311,-7.99122327230096));
#10292=CARTESIAN_POINT('Ctrl Pts',(4.02836682984751,312.001074056311,-6.911825633427));
#10293=CARTESIAN_POINT('Ctrl Pts',(5.88038492654901,312.138574056311,-5.83242799455303));
#10294=CARTESIAN_POINT('Ctrl Pts',(6.94458082712403,312.276074056311,-3.9716331701525));
#10295=CARTESIAN_POINT('Ctrl Pts',(8.00877672769905,312.413574056311,-2.11083834575195));
#10296=CARTESIAN_POINT('Ctrl Pts',(8.,312.551074056311,0.0327551936970304));
#10297=CARTESIAN_POINT('Ctrl Pts',(7.99122327230096,312.688574056311,2.17634873314601));
#10298=CARTESIAN_POINT('Ctrl Pts',(6.911825633427,312.826074056311,4.02836682984751));
#10299=CARTESIAN_POINT('Ctrl Pts',(5.83242799455304,312.963574056311,5.880384926549));
#10300=CARTESIAN_POINT('Ctrl Pts',(3.9716331701525,313.101074056311,6.94458082712403));
#10301=CARTESIAN_POINT('Ctrl Pts',(2.11083834575196,313.238574056311,8.00877672769905));
#10302=CARTESIAN_POINT('Ctrl Pts',(-0.0327551936970299,313.376074056311,
8.));
#10303=CARTESIAN_POINT('Ctrl Pts',(-2.17634873314601,313.513574056311,7.99122327230096));
#10304=CARTESIAN_POINT('Ctrl Pts',(-4.02836682984751,313.651074056311,6.911825633427));
#10305=CARTESIAN_POINT('Ctrl Pts',(-5.88038492654901,313.788574056311,5.83242799455303));
#10306=CARTESIAN_POINT('Ctrl Pts',(-6.94458082712403,313.926074056311,3.9716331701525));
#10307=CARTESIAN_POINT('Ctrl Pts',(-8.00877672769905,314.063574056311,2.11083834575196));
#10308=CARTESIAN_POINT('Ctrl Pts',(-8.,314.201074056311,-0.0327551936970314));
#10309=CARTESIAN_POINT('Ctrl Pts',(-7.99122327230096,314.338574056311,-2.17634873314601));
#10310=CARTESIAN_POINT('Ctrl Pts',(-6.911825633427,314.476074056311,-4.02836682984751));
#10311=CARTESIAN_POINT('Ctrl Pts',(-5.83242799455303,314.613574056311,-5.88038492654901));
#10312=CARTESIAN_POINT('Ctrl Pts',(-3.97163317015249,314.751074056311,-6.94458082712403));
#10313=CARTESIAN_POINT('Ctrl Pts',(-2.11083834575195,314.888574056311,-8.00877672769905));
#10314=CARTESIAN_POINT('Ctrl Pts',(0.0327551936970309,315.026074056311,
-8.));
#10315=CARTESIAN_POINT('Ctrl Pts',(2.17634873314601,315.163574056311,-7.99122327230096));
#10316=CARTESIAN_POINT('Ctrl Pts',(4.02836682984751,315.301074056311,-6.911825633427));
#10317=CARTESIAN_POINT('Ctrl Pts',(5.88038492654901,315.438574056311,-5.83242799455303));
#10318=CARTESIAN_POINT('Ctrl Pts',(6.94458082712403,315.576074056311,-3.9716331701525));
#10319=CARTESIAN_POINT('Ctrl Pts',(8.00877672769905,315.713574056311,-2.11083834575195));
#10320=CARTESIAN_POINT('Ctrl Pts',(8.,315.851074056311,0.0327551936970304));
#10321=CARTESIAN_POINT('Ctrl Pts',(7.99122327230096,315.988574056311,2.17634873314601));
#10322=CARTESIAN_POINT('Ctrl Pts',(6.911825633427,316.126074056311,4.02836682984751));
#10323=CARTESIAN_POINT('Ctrl Pts',(5.83242799455304,316.263574056311,5.880384926549));
#10324=CARTESIAN_POINT('Ctrl Pts',(3.9716331701525,316.401074056311,6.94458082712403));
#10325=CARTESIAN_POINT('Ctrl Pts',(2.11083834575196,316.538574056311,8.00877672769905));
#10326=CARTESIAN_POINT('Ctrl Pts',(-0.0327551936970299,316.676074056311,
8.));
#10327=CARTESIAN_POINT('Ctrl Pts',(-2.17634873314601,316.813574056311,7.99122327230096));
#10328=CARTESIAN_POINT('Ctrl Pts',(-4.02836682984751,316.951074056311,6.911825633427));
#10329=CARTESIAN_POINT('Ctrl Pts',(-5.88038492654901,317.088574056311,5.83242799455303));
#10330=CARTESIAN_POINT('Ctrl Pts',(-6.94458082712403,317.226074056311,3.9716331701525));
#10331=CARTESIAN_POINT('Ctrl Pts',(-8.00877672769905,317.363574056311,2.11083834575196));
#10332=CARTESIAN_POINT('Ctrl Pts',(-8.,317.501074056311,-0.0327551936970314));
#10333=CARTESIAN_POINT('Ctrl Pts',(-9.,284.501074056311,-0.0327551936970214));
#10334=CARTESIAN_POINT('Ctrl Pts',(-8.99122327230096,284.638574056311,-2.44429792557713));
#10335=CARTESIAN_POINT('Ctrl Pts',(-7.77785103721144,284.776074056311,-4.5283668298475));
#10336=CARTESIAN_POINT('Ctrl Pts',(-6.56447880212192,284.913574056311,-6.61243573411788));
#10337=CARTESIAN_POINT('Ctrl Pts',(-4.4716331701525,285.051074056311,-7.81060623090846));
#10338=CARTESIAN_POINT('Ctrl Pts',(-2.37878753818309,285.188574056311,-9.00877672769904));
#10339=CARTESIAN_POINT('Ctrl Pts',(0.0327551936970209,285.326074056311,
-9.));
#10340=CARTESIAN_POINT('Ctrl Pts',(2.44429792557713,285.463574056311,-8.99122327230096));
#10341=CARTESIAN_POINT('Ctrl Pts',(4.5283668298475,285.601074056311,-7.77785103721144));
#10342=CARTESIAN_POINT('Ctrl Pts',(6.61243573411788,285.738574056311,-6.56447880212192));
#10343=CARTESIAN_POINT('Ctrl Pts',(7.81060623090846,285.876074056311,-4.4716331701525));
#10344=CARTESIAN_POINT('Ctrl Pts',(9.00877672769904,286.013574056311,-2.37878753818309));
#10345=CARTESIAN_POINT('Ctrl Pts',(9.,286.151074056311,0.0327551936970203));
#10346=CARTESIAN_POINT('Ctrl Pts',(8.99122327230096,286.288574056311,2.44429792557712));
#10347=CARTESIAN_POINT('Ctrl Pts',(7.77785103721144,286.426074056311,4.5283668298475));
#10348=CARTESIAN_POINT('Ctrl Pts',(6.56447880212192,286.563574056311,6.61243573411788));
#10349=CARTESIAN_POINT('Ctrl Pts',(4.47163317015251,286.701074056311,7.81060623090846));
#10350=CARTESIAN_POINT('Ctrl Pts',(2.37878753818309,286.838574056311,9.00877672769904));
#10351=CARTESIAN_POINT('Ctrl Pts',(-0.0327551936970198,286.976074056311,
9.));
#10352=CARTESIAN_POINT('Ctrl Pts',(-2.44429792557712,287.113574056311,8.99122327230096));
#10353=CARTESIAN_POINT('Ctrl Pts',(-4.5283668298475,287.251074056311,7.77785103721144));
#10354=CARTESIAN_POINT('Ctrl Pts',(-6.61243573411788,287.388574056311,6.56447880212192));
#10355=CARTESIAN_POINT('Ctrl Pts',(-7.81060623090846,287.526074056311,4.47163317015251));
#10356=CARTESIAN_POINT('Ctrl Pts',(-9.00877672769904,287.663574056311,2.37878753818309));
#10357=CARTESIAN_POINT('Ctrl Pts',(-9.,287.801074056311,-0.0327551936970214));
#10358=CARTESIAN_POINT('Ctrl Pts',(-8.99122327230096,287.938574056311,-2.44429792557713));
#10359=CARTESIAN_POINT('Ctrl Pts',(-7.77785103721144,288.076074056311,-4.5283668298475));
#10360=CARTESIAN_POINT('Ctrl Pts',(-6.56447880212192,288.213574056311,-6.61243573411788));
#10361=CARTESIAN_POINT('Ctrl Pts',(-4.4716331701525,288.351074056311,-7.81060623090846));
#10362=CARTESIAN_POINT('Ctrl Pts',(-2.37878753818309,288.488574056311,-9.00877672769904));
#10363=CARTESIAN_POINT('Ctrl Pts',(0.0327551936970209,288.626074056311,
-9.));
#10364=CARTESIAN_POINT('Ctrl Pts',(2.44429792557713,288.763574056311,-8.99122327230096));
#10365=CARTESIAN_POINT('Ctrl Pts',(4.5283668298475,288.901074056311,-7.77785103721144));
#10366=CARTESIAN_POINT('Ctrl Pts',(6.61243573411788,289.038574056311,-6.56447880212192));
#10367=CARTESIAN_POINT('Ctrl Pts',(7.81060623090846,289.176074056311,-4.4716331701525));
#10368=CARTESIAN_POINT('Ctrl Pts',(9.00877672769904,289.313574056311,-2.37878753818309));
#10369=CARTESIAN_POINT('Ctrl Pts',(9.,289.451074056311,0.0327551936970203));
#10370=CARTESIAN_POINT('Ctrl Pts',(8.99122327230096,289.588574056311,2.44429792557712));
#10371=CARTESIAN_POINT('Ctrl Pts',(7.77785103721144,289.726074056311,4.5283668298475));
#10372=CARTESIAN_POINT('Ctrl Pts',(6.56447880212192,289.863574056311,6.61243573411788));
#10373=CARTESIAN_POINT('Ctrl Pts',(4.47163317015251,290.001074056311,7.81060623090846));
#10374=CARTESIAN_POINT('Ctrl Pts',(2.37878753818309,290.138574056311,9.00877672769904));
#10375=CARTESIAN_POINT('Ctrl Pts',(-0.0327551936970198,290.276074056311,
9.));
#10376=CARTESIAN_POINT('Ctrl Pts',(-2.44429792557712,290.413574056311,8.99122327230096));
#10377=CARTESIAN_POINT('Ctrl Pts',(-4.5283668298475,290.551074056311,7.77785103721144));
#10378=CARTESIAN_POINT('Ctrl Pts',(-6.61243573411788,290.688574056311,6.56447880212192));
#10379=CARTESIAN_POINT('Ctrl Pts',(-7.81060623090846,290.826074056311,4.47163317015251));
#10380=CARTESIAN_POINT('Ctrl Pts',(-9.00877672769904,290.963574056311,2.37878753818309));
#10381=CARTESIAN_POINT('Ctrl Pts',(-9.,291.101074056311,-0.0327551936970214));
#10382=CARTESIAN_POINT('Ctrl Pts',(-8.99122327230096,291.238574056311,-2.44429792557713));
#10383=CARTESIAN_POINT('Ctrl Pts',(-7.77785103721144,291.376074056311,-4.5283668298475));
#10384=CARTESIAN_POINT('Ctrl Pts',(-6.56447880212192,291.513574056311,-6.61243573411788));
#10385=CARTESIAN_POINT('Ctrl Pts',(-4.4716331701525,291.651074056311,-7.81060623090846));
#10386=CARTESIAN_POINT('Ctrl Pts',(-2.37878753818309,291.788574056311,-9.00877672769904));
#10387=CARTESIAN_POINT('Ctrl Pts',(0.0327551936970209,291.926074056311,
-9.));
#10388=CARTESIAN_POINT('Ctrl Pts',(2.44429792557713,292.063574056311,-8.99122327230096));
#10389=CARTESIAN_POINT('Ctrl Pts',(4.5283668298475,292.201074056311,-7.77785103721144));
#10390=CARTESIAN_POINT('Ctrl Pts',(6.61243573411788,292.338574056311,-6.56447880212192));
#10391=CARTESIAN_POINT('Ctrl Pts',(7.81060623090846,292.476074056311,-4.4716331701525));
#10392=CARTESIAN_POINT('Ctrl Pts',(9.00877672769904,292.613574056311,-2.37878753818309));
#10393=CARTESIAN_POINT('Ctrl Pts',(9.,292.751074056311,0.0327551936970203));
#10394=CARTESIAN_POINT('Ctrl Pts',(8.99122327230096,292.888574056311,2.44429792557712));
#10395=CARTESIAN_POINT('Ctrl Pts',(7.77785103721144,293.026074056311,4.5283668298475));
#10396=CARTESIAN_POINT('Ctrl Pts',(6.56447880212192,293.163574056311,6.61243573411788));
#10397=CARTESIAN_POINT('Ctrl Pts',(4.47163317015251,293.301074056311,7.81060623090846));
#10398=CARTESIAN_POINT('Ctrl Pts',(2.37878753818309,293.438574056311,9.00877672769904));
#10399=CARTESIAN_POINT('Ctrl Pts',(-0.0327551936970198,293.576074056311,
9.));
#10400=CARTESIAN_POINT('Ctrl Pts',(-2.44429792557712,293.713574056311,8.99122327230096));
#10401=CARTESIAN_POINT('Ctrl Pts',(-4.5283668298475,293.851074056311,7.77785103721144));
#10402=CARTESIAN_POINT('Ctrl Pts',(-6.61243573411788,293.988574056311,6.56447880212192));
#10403=CARTESIAN_POINT('Ctrl Pts',(-7.81060623090846,294.126074056311,4.47163317015251));
#10404=CARTESIAN_POINT('Ctrl Pts',(-9.00877672769904,294.263574056311,2.37878753818309));
#10405=CARTESIAN_POINT('Ctrl Pts',(-9.,294.401074056311,-0.0327551936970214));
#10406=CARTESIAN_POINT('Ctrl Pts',(-8.99122327230096,294.538574056311,-2.44429792557713));
#10407=CARTESIAN_POINT('Ctrl Pts',(-7.77785103721144,294.676074056311,-4.5283668298475));
#10408=CARTESIAN_POINT('Ctrl Pts',(-6.56447880212192,294.813574056311,-6.61243573411788));
#10409=CARTESIAN_POINT('Ctrl Pts',(-4.4716331701525,294.951074056311,-7.81060623090846));
#10410=CARTESIAN_POINT('Ctrl Pts',(-2.37878753818309,295.088574056311,-9.00877672769904));
#10411=CARTESIAN_POINT('Ctrl Pts',(0.0327551936970209,295.226074056311,
-9.));
#10412=CARTESIAN_POINT('Ctrl Pts',(2.44429792557713,295.363574056311,-8.99122327230096));
#10413=CARTESIAN_POINT('Ctrl Pts',(4.5283668298475,295.501074056311,-7.77785103721144));
#10414=CARTESIAN_POINT('Ctrl Pts',(6.61243573411788,295.638574056311,-6.56447880212192));
#10415=CARTESIAN_POINT('Ctrl Pts',(7.81060623090846,295.776074056311,-4.4716331701525));
#10416=CARTESIAN_POINT('Ctrl Pts',(9.00877672769904,295.913574056311,-2.37878753818309));
#10417=CARTESIAN_POINT('Ctrl Pts',(9.,296.051074056311,0.0327551936970203));
#10418=CARTESIAN_POINT('Ctrl Pts',(8.99122327230096,296.188574056311,2.44429792557712));
#10419=CARTESIAN_POINT('Ctrl Pts',(7.77785103721144,296.326074056311,4.5283668298475));
#10420=CARTESIAN_POINT('Ctrl Pts',(6.56447880212192,296.463574056311,6.61243573411788));
#10421=CARTESIAN_POINT('Ctrl Pts',(4.47163317015251,296.601074056311,7.81060623090846));
#10422=CARTESIAN_POINT('Ctrl Pts',(2.37878753818309,296.738574056311,9.00877672769904));
#10423=CARTESIAN_POINT('Ctrl Pts',(-0.0327551936970198,296.876074056311,
9.));
#10424=CARTESIAN_POINT('Ctrl Pts',(-2.44429792557712,297.013574056311,8.99122327230096));
#10425=CARTESIAN_POINT('Ctrl Pts',(-4.5283668298475,297.151074056311,7.77785103721144));
#10426=CARTESIAN_POINT('Ctrl Pts',(-6.61243573411788,297.288574056311,6.56447880212192));
#10427=CARTESIAN_POINT('Ctrl Pts',(-7.81060623090846,297.426074056311,4.47163317015251));
#10428=CARTESIAN_POINT('Ctrl Pts',(-9.00877672769904,297.563574056311,2.37878753818309));
#10429=CARTESIAN_POINT('Ctrl Pts',(-9.,297.701074056311,-0.0327551936970214));
#10430=CARTESIAN_POINT('Ctrl Pts',(-8.99122327230096,297.838574056311,-2.44429792557713));
#10431=CARTESIAN_POINT('Ctrl Pts',(-7.77785103721144,297.976074056311,-4.5283668298475));
#10432=CARTESIAN_POINT('Ctrl Pts',(-6.56447880212192,298.113574056311,-6.61243573411788));
#10433=CARTESIAN_POINT('Ctrl Pts',(-4.4716331701525,298.251074056311,-7.81060623090846));
#10434=CARTESIAN_POINT('Ctrl Pts',(-2.37878753818309,298.388574056311,-9.00877672769904));
#10435=CARTESIAN_POINT('Ctrl Pts',(0.0327551936970209,298.526074056311,
-9.));
#10436=CARTESIAN_POINT('Ctrl Pts',(2.44429792557713,298.663574056311,-8.99122327230096));
#10437=CARTESIAN_POINT('Ctrl Pts',(4.5283668298475,298.801074056311,-7.77785103721144));
#10438=CARTESIAN_POINT('Ctrl Pts',(6.61243573411788,298.938574056311,-6.56447880212192));
#10439=CARTESIAN_POINT('Ctrl Pts',(7.81060623090846,299.076074056311,-4.4716331701525));
#10440=CARTESIAN_POINT('Ctrl Pts',(9.00877672769904,299.213574056311,-2.37878753818309));
#10441=CARTESIAN_POINT('Ctrl Pts',(9.,299.351074056311,0.0327551936970203));
#10442=CARTESIAN_POINT('Ctrl Pts',(8.99122327230096,299.488574056311,2.44429792557712));
#10443=CARTESIAN_POINT('Ctrl Pts',(7.77785103721144,299.626074056311,4.5283668298475));
#10444=CARTESIAN_POINT('Ctrl Pts',(6.56447880212192,299.763574056311,6.61243573411788));
#10445=CARTESIAN_POINT('Ctrl Pts',(4.47163317015251,299.901074056311,7.81060623090846));
#10446=CARTESIAN_POINT('Ctrl Pts',(2.37878753818309,300.038574056311,9.00877672769904));
#10447=CARTESIAN_POINT('Ctrl Pts',(-0.0327551936970198,300.176074056311,
9.));
#10448=CARTESIAN_POINT('Ctrl Pts',(-2.44429792557712,300.313574056311,8.99122327230096));
#10449=CARTESIAN_POINT('Ctrl Pts',(-4.5283668298475,300.451074056311,7.77785103721144));
#10450=CARTESIAN_POINT('Ctrl Pts',(-6.61243573411788,300.588574056311,6.56447880212192));
#10451=CARTESIAN_POINT('Ctrl Pts',(-7.81060623090846,300.726074056311,4.47163317015251));
#10452=CARTESIAN_POINT('Ctrl Pts',(-9.00877672769904,300.863574056311,2.37878753818309));
#10453=CARTESIAN_POINT('Ctrl Pts',(-9.,301.001074056311,-0.0327551936970214));
#10454=CARTESIAN_POINT('Ctrl Pts',(-8.99122327230096,301.138574056311,-2.44429792557713));
#10455=CARTESIAN_POINT('Ctrl Pts',(-7.77785103721144,301.276074056311,-4.5283668298475));
#10456=CARTESIAN_POINT('Ctrl Pts',(-6.56447880212192,301.413574056311,-6.61243573411788));
#10457=CARTESIAN_POINT('Ctrl Pts',(-4.4716331701525,301.551074056311,-7.81060623090846));
#10458=CARTESIAN_POINT('Ctrl Pts',(-2.37878753818309,301.688574056311,-9.00877672769904));
#10459=CARTESIAN_POINT('Ctrl Pts',(0.0327551936970209,301.826074056311,
-9.));
#10460=CARTESIAN_POINT('Ctrl Pts',(2.44429792557713,301.963574056311,-8.99122327230096));
#10461=CARTESIAN_POINT('Ctrl Pts',(4.5283668298475,302.101074056311,-7.77785103721144));
#10462=CARTESIAN_POINT('Ctrl Pts',(6.61243573411788,302.238574056311,-6.56447880212192));
#10463=CARTESIAN_POINT('Ctrl Pts',(7.81060623090846,302.376074056311,-4.4716331701525));
#10464=CARTESIAN_POINT('Ctrl Pts',(9.00877672769904,302.513574056311,-2.37878753818309));
#10465=CARTESIAN_POINT('Ctrl Pts',(9.,302.651074056311,0.0327551936970203));
#10466=CARTESIAN_POINT('Ctrl Pts',(8.99122327230096,302.788574056311,2.44429792557712));
#10467=CARTESIAN_POINT('Ctrl Pts',(7.77785103721144,302.926074056311,4.5283668298475));
#10468=CARTESIAN_POINT('Ctrl Pts',(6.56447880212192,303.063574056311,6.61243573411788));
#10469=CARTESIAN_POINT('Ctrl Pts',(4.47163317015251,303.201074056311,7.81060623090846));
#10470=CARTESIAN_POINT('Ctrl Pts',(2.37878753818309,303.338574056311,9.00877672769904));
#10471=CARTESIAN_POINT('Ctrl Pts',(-0.0327551936970198,303.476074056311,
9.));
#10472=CARTESIAN_POINT('Ctrl Pts',(-2.44429792557712,303.613574056311,8.99122327230096));
#10473=CARTESIAN_POINT('Ctrl Pts',(-4.5283668298475,303.751074056311,7.77785103721144));
#10474=CARTESIAN_POINT('Ctrl Pts',(-6.61243573411788,303.888574056311,6.56447880212192));
#10475=CARTESIAN_POINT('Ctrl Pts',(-7.81060623090846,304.026074056311,4.47163317015251));
#10476=CARTESIAN_POINT('Ctrl Pts',(-9.00877672769904,304.163574056311,2.37878753818309));
#10477=CARTESIAN_POINT('Ctrl Pts',(-9.,304.301074056311,-0.0327551936970214));
#10478=CARTESIAN_POINT('Ctrl Pts',(-8.99122327230096,304.438574056311,-2.44429792557713));
#10479=CARTESIAN_POINT('Ctrl Pts',(-7.77785103721144,304.576074056311,-4.5283668298475));
#10480=CARTESIAN_POINT('Ctrl Pts',(-6.56447880212192,304.713574056311,-6.61243573411788));
#10481=CARTESIAN_POINT('Ctrl Pts',(-4.4716331701525,304.851074056311,-7.81060623090846));
#10482=CARTESIAN_POINT('Ctrl Pts',(-2.37878753818309,304.988574056311,-9.00877672769904));
#10483=CARTESIAN_POINT('Ctrl Pts',(0.0327551936970209,305.126074056311,
-9.));
#10484=CARTESIAN_POINT('Ctrl Pts',(2.44429792557713,305.263574056311,-8.99122327230096));
#10485=CARTESIAN_POINT('Ctrl Pts',(4.5283668298475,305.401074056311,-7.77785103721144));
#10486=CARTESIAN_POINT('Ctrl Pts',(6.61243573411788,305.538574056311,-6.56447880212192));
#10487=CARTESIAN_POINT('Ctrl Pts',(7.81060623090846,305.676074056311,-4.4716331701525));
#10488=CARTESIAN_POINT('Ctrl Pts',(9.00877672769904,305.813574056311,-2.37878753818309));
#10489=CARTESIAN_POINT('Ctrl Pts',(9.,305.951074056311,0.0327551936970203));
#10490=CARTESIAN_POINT('Ctrl Pts',(8.99122327230096,306.088574056311,2.44429792557712));
#10491=CARTESIAN_POINT('Ctrl Pts',(7.77785103721144,306.226074056311,4.5283668298475));
#10492=CARTESIAN_POINT('Ctrl Pts',(6.56447880212192,306.363574056311,6.61243573411788));
#10493=CARTESIAN_POINT('Ctrl Pts',(4.47163317015251,306.501074056311,7.81060623090846));
#10494=CARTESIAN_POINT('Ctrl Pts',(2.37878753818309,306.638574056311,9.00877672769904));
#10495=CARTESIAN_POINT('Ctrl Pts',(-0.0327551936970198,306.776074056311,
9.));
#10496=CARTESIAN_POINT('Ctrl Pts',(-2.44429792557712,306.913574056311,8.99122327230096));
#10497=CARTESIAN_POINT('Ctrl Pts',(-4.5283668298475,307.051074056311,7.77785103721144));
#10498=CARTESIAN_POINT('Ctrl Pts',(-6.61243573411788,307.188574056311,6.56447880212192));
#10499=CARTESIAN_POINT('Ctrl Pts',(-7.81060623090846,307.326074056311,4.47163317015251));
#10500=CARTESIAN_POINT('Ctrl Pts',(-9.00877672769904,307.463574056311,2.37878753818309));
#10501=CARTESIAN_POINT('Ctrl Pts',(-9.,307.601074056311,-0.0327551936970214));
#10502=CARTESIAN_POINT('Ctrl Pts',(-8.99122327230096,307.738574056311,-2.44429792557713));
#10503=CARTESIAN_POINT('Ctrl Pts',(-7.77785103721144,307.876074056311,-4.5283668298475));
#10504=CARTESIAN_POINT('Ctrl Pts',(-6.56447880212192,308.013574056311,-6.61243573411788));
#10505=CARTESIAN_POINT('Ctrl Pts',(-4.4716331701525,308.151074056311,-7.81060623090846));
#10506=CARTESIAN_POINT('Ctrl Pts',(-2.37878753818309,308.288574056311,-9.00877672769904));
#10507=CARTESIAN_POINT('Ctrl Pts',(0.0327551936970209,308.426074056311,
-9.));
#10508=CARTESIAN_POINT('Ctrl Pts',(2.44429792557713,308.563574056311,-8.99122327230096));
#10509=CARTESIAN_POINT('Ctrl Pts',(4.5283668298475,308.701074056311,-7.77785103721144));
#10510=CARTESIAN_POINT('Ctrl Pts',(6.61243573411788,308.838574056311,-6.56447880212192));
#10511=CARTESIAN_POINT('Ctrl Pts',(7.81060623090846,308.976074056311,-4.4716331701525));
#10512=CARTESIAN_POINT('Ctrl Pts',(9.00877672769904,309.113574056311,-2.37878753818309));
#10513=CARTESIAN_POINT('Ctrl Pts',(9.,309.251074056311,0.0327551936970203));
#10514=CARTESIAN_POINT('Ctrl Pts',(8.99122327230096,309.388574056311,2.44429792557712));
#10515=CARTESIAN_POINT('Ctrl Pts',(7.77785103721144,309.526074056311,4.5283668298475));
#10516=CARTESIAN_POINT('Ctrl Pts',(6.56447880212192,309.663574056311,6.61243573411788));
#10517=CARTESIAN_POINT('Ctrl Pts',(4.47163317015251,309.801074056311,7.81060623090846));
#10518=CARTESIAN_POINT('Ctrl Pts',(2.37878753818309,309.938574056311,9.00877672769904));
#10519=CARTESIAN_POINT('Ctrl Pts',(-0.0327551936970198,310.076074056311,
9.));
#10520=CARTESIAN_POINT('Ctrl Pts',(-2.44429792557712,310.213574056311,8.99122327230096));
#10521=CARTESIAN_POINT('Ctrl Pts',(-4.5283668298475,310.351074056311,7.77785103721144));
#10522=CARTESIAN_POINT('Ctrl Pts',(-6.61243573411788,310.488574056311,6.56447880212192));
#10523=CARTESIAN_POINT('Ctrl Pts',(-7.81060623090846,310.626074056311,4.47163317015251));
#10524=CARTESIAN_POINT('Ctrl Pts',(-9.00877672769904,310.763574056311,2.37878753818309));
#10525=CARTESIAN_POINT('Ctrl Pts',(-9.,310.901074056311,-0.0327551936970214));
#10526=CARTESIAN_POINT('Ctrl Pts',(-8.99122327230096,311.038574056311,-2.44429792557713));
#10527=CARTESIAN_POINT('Ctrl Pts',(-7.77785103721144,311.176074056311,-4.5283668298475));
#10528=CARTESIAN_POINT('Ctrl Pts',(-6.56447880212192,311.313574056311,-6.61243573411788));
#10529=CARTESIAN_POINT('Ctrl Pts',(-4.4716331701525,311.451074056311,-7.81060623090846));
#10530=CARTESIAN_POINT('Ctrl Pts',(-2.37878753818309,311.588574056311,-9.00877672769904));
#10531=CARTESIAN_POINT('Ctrl Pts',(0.0327551936970209,311.726074056311,
-9.));
#10532=CARTESIAN_POINT('Ctrl Pts',(2.44429792557713,311.863574056311,-8.99122327230096));
#10533=CARTESIAN_POINT('Ctrl Pts',(4.5283668298475,312.001074056311,-7.77785103721144));
#10534=CARTESIAN_POINT('Ctrl Pts',(6.61243573411788,312.138574056311,-6.56447880212192));
#10535=CARTESIAN_POINT('Ctrl Pts',(7.81060623090846,312.276074056311,-4.4716331701525));
#10536=CARTESIAN_POINT('Ctrl Pts',(9.00877672769904,312.413574056311,-2.37878753818309));
#10537=CARTESIAN_POINT('Ctrl Pts',(9.,312.551074056311,0.0327551936970203));
#10538=CARTESIAN_POINT('Ctrl Pts',(8.99122327230096,312.688574056311,2.44429792557712));
#10539=CARTESIAN_POINT('Ctrl Pts',(7.77785103721144,312.826074056311,4.5283668298475));
#10540=CARTESIAN_POINT('Ctrl Pts',(6.56447880212192,312.963574056311,6.61243573411788));
#10541=CARTESIAN_POINT('Ctrl Pts',(4.47163317015251,313.101074056311,7.81060623090846));
#10542=CARTESIAN_POINT('Ctrl Pts',(2.37878753818309,313.238574056311,9.00877672769904));
#10543=CARTESIAN_POINT('Ctrl Pts',(-0.0327551936970198,313.376074056311,
9.));
#10544=CARTESIAN_POINT('Ctrl Pts',(-2.44429792557712,313.513574056311,8.99122327230096));
#10545=CARTESIAN_POINT('Ctrl Pts',(-4.5283668298475,313.651074056311,7.77785103721144));
#10546=CARTESIAN_POINT('Ctrl Pts',(-6.61243573411788,313.788574056311,6.56447880212192));
#10547=CARTESIAN_POINT('Ctrl Pts',(-7.81060623090846,313.926074056311,4.47163317015251));
#10548=CARTESIAN_POINT('Ctrl Pts',(-9.00877672769904,314.063574056311,2.37878753818309));
#10549=CARTESIAN_POINT('Ctrl Pts',(-9.,314.201074056311,-0.0327551936970214));
#10550=CARTESIAN_POINT('Ctrl Pts',(-8.99122327230096,314.338574056311,-2.44429792557713));
#10551=CARTESIAN_POINT('Ctrl Pts',(-7.77785103721144,314.476074056311,-4.5283668298475));
#10552=CARTESIAN_POINT('Ctrl Pts',(-6.56447880212192,314.613574056311,-6.61243573411788));
#10553=CARTESIAN_POINT('Ctrl Pts',(-4.4716331701525,314.751074056311,-7.81060623090846));
#10554=CARTESIAN_POINT('Ctrl Pts',(-2.37878753818309,314.888574056311,-9.00877672769904));
#10555=CARTESIAN_POINT('Ctrl Pts',(0.0327551936970209,315.026074056311,
-9.));
#10556=CARTESIAN_POINT('Ctrl Pts',(2.44429792557713,315.163574056311,-8.99122327230096));
#10557=CARTESIAN_POINT('Ctrl Pts',(4.5283668298475,315.301074056311,-7.77785103721144));
#10558=CARTESIAN_POINT('Ctrl Pts',(6.61243573411788,315.438574056311,-6.56447880212192));
#10559=CARTESIAN_POINT('Ctrl Pts',(7.81060623090846,315.576074056311,-4.4716331701525));
#10560=CARTESIAN_POINT('Ctrl Pts',(9.00877672769904,315.713574056311,-2.37878753818309));
#10561=CARTESIAN_POINT('Ctrl Pts',(9.,315.851074056311,0.0327551936970203));
#10562=CARTESIAN_POINT('Ctrl Pts',(8.99122327230096,315.988574056311,2.44429792557712));
#10563=CARTESIAN_POINT('Ctrl Pts',(7.77785103721144,316.126074056311,4.5283668298475));
#10564=CARTESIAN_POINT('Ctrl Pts',(6.56447880212192,316.263574056311,6.61243573411788));
#10565=CARTESIAN_POINT('Ctrl Pts',(4.47163317015251,316.401074056311,7.81060623090846));
#10566=CARTESIAN_POINT('Ctrl Pts',(2.37878753818309,316.538574056311,9.00877672769904));
#10567=CARTESIAN_POINT('Ctrl Pts',(-0.0327551936970198,316.676074056311,
9.));
#10568=CARTESIAN_POINT('Ctrl Pts',(-2.44429792557712,316.813574056311,8.99122327230096));
#10569=CARTESIAN_POINT('Ctrl Pts',(-4.5283668298475,316.951074056311,7.77785103721144));
#10570=CARTESIAN_POINT('Ctrl Pts',(-6.61243573411788,317.088574056311,6.56447880212192));
#10571=CARTESIAN_POINT('Ctrl Pts',(-7.81060623090846,317.226074056311,4.47163317015251));
#10572=CARTESIAN_POINT('Ctrl Pts',(-9.00877672769904,317.363574056311,2.37878753818309));
#10573=CARTESIAN_POINT('Ctrl Pts',(-9.,317.501074056311,-0.0327551936970214));
#10574=CARTESIAN_POINT('Ctrl Pts',(-9.,285.498925943689,0.0327551936972079));
#10575=CARTESIAN_POINT('Ctrl Pts',(-9.0087767276991,285.636425943689,-2.3787875381829));
#10576=CARTESIAN_POINT('Ctrl Pts',(-7.81060623090856,285.773925943689,-4.47163317015234));
#10577=CARTESIAN_POINT('Ctrl Pts',(-6.61243573411802,285.911425943689,-6.56447880212179));
#10578=CARTESIAN_POINT('Ctrl Pts',(-4.52836682984766,286.048925943689,-7.77785103721135));
#10579=CARTESIAN_POINT('Ctrl Pts',(-2.44429792557731,286.186425943689,-8.99122327230091));
#10580=CARTESIAN_POINT('Ctrl Pts',(-0.0327551936972084,286.323925943689,
-9.));
#10581=CARTESIAN_POINT('Ctrl Pts',(2.3787875381829,286.461425943689,-9.0087767276991));
#10582=CARTESIAN_POINT('Ctrl Pts',(4.47163317015234,286.598925943689,-7.81060623090856));
#10583=CARTESIAN_POINT('Ctrl Pts',(6.56447880212178,286.736425943689,-6.61243573411802));
#10584=CARTESIAN_POINT('Ctrl Pts',(7.77785103721135,286.873925943689,-4.52836682984767));
#10585=CARTESIAN_POINT('Ctrl Pts',(8.99122327230091,287.011425943689,-2.44429792557732));
#10586=CARTESIAN_POINT('Ctrl Pts',(9.,287.148925943689,-0.032755193697209));
#10587=CARTESIAN_POINT('Ctrl Pts',(9.0087767276991,287.286425943689,2.37878753818289));
#10588=CARTESIAN_POINT('Ctrl Pts',(7.81060623090856,287.423925943689,4.47163317015234));
#10589=CARTESIAN_POINT('Ctrl Pts',(6.61243573411802,287.561425943689,6.56447880212178));
#10590=CARTESIAN_POINT('Ctrl Pts',(4.52836682984767,287.698925943689,7.77785103721135));
#10591=CARTESIAN_POINT('Ctrl Pts',(2.44429792557732,287.836425943689,8.99122327230091));
#10592=CARTESIAN_POINT('Ctrl Pts',(0.0327551936972095,287.973925943689,
9.));
#10593=CARTESIAN_POINT('Ctrl Pts',(-2.37878753818289,288.111425943689,9.0087767276991));
#10594=CARTESIAN_POINT('Ctrl Pts',(-4.47163317015233,288.248925943689,7.81060623090856));
#10595=CARTESIAN_POINT('Ctrl Pts',(-6.56447880212178,288.386425943689,6.61243573411802));
#10596=CARTESIAN_POINT('Ctrl Pts',(-7.77785103721135,288.523925943689,4.52836682984767));
#10597=CARTESIAN_POINT('Ctrl Pts',(-8.99122327230091,288.661425943689,2.44429792557732));
#10598=CARTESIAN_POINT('Ctrl Pts',(-9.,288.798925943689,0.0327551936972079));
#10599=CARTESIAN_POINT('Ctrl Pts',(-9.0087767276991,288.936425943689,-2.3787875381829));
#10600=CARTESIAN_POINT('Ctrl Pts',(-7.81060623090856,289.073925943689,-4.47163317015234));
#10601=CARTESIAN_POINT('Ctrl Pts',(-6.61243573411802,289.211425943689,-6.56447880212179));
#10602=CARTESIAN_POINT('Ctrl Pts',(-4.52836682984766,289.348925943689,-7.77785103721135));
#10603=CARTESIAN_POINT('Ctrl Pts',(-2.44429792557731,289.486425943689,-8.99122327230091));
#10604=CARTESIAN_POINT('Ctrl Pts',(-0.0327551936972084,289.623925943689,
-9.));
#10605=CARTESIAN_POINT('Ctrl Pts',(2.3787875381829,289.761425943689,-9.0087767276991));
#10606=CARTESIAN_POINT('Ctrl Pts',(4.47163317015234,289.898925943689,-7.81060623090856));
#10607=CARTESIAN_POINT('Ctrl Pts',(6.56447880212178,290.036425943689,-6.61243573411802));
#10608=CARTESIAN_POINT('Ctrl Pts',(7.77785103721135,290.173925943689,-4.52836682984767));
#10609=CARTESIAN_POINT('Ctrl Pts',(8.99122327230091,290.311425943689,-2.44429792557732));
#10610=CARTESIAN_POINT('Ctrl Pts',(9.,290.448925943689,-0.032755193697209));
#10611=CARTESIAN_POINT('Ctrl Pts',(9.0087767276991,290.586425943689,2.37878753818289));
#10612=CARTESIAN_POINT('Ctrl Pts',(7.81060623090856,290.723925943689,4.47163317015234));
#10613=CARTESIAN_POINT('Ctrl Pts',(6.61243573411802,290.861425943689,6.56447880212178));
#10614=CARTESIAN_POINT('Ctrl Pts',(4.52836682984767,290.998925943689,7.77785103721135));
#10615=CARTESIAN_POINT('Ctrl Pts',(2.44429792557732,291.136425943689,8.99122327230091));
#10616=CARTESIAN_POINT('Ctrl Pts',(0.0327551936972095,291.273925943689,
9.));
#10617=CARTESIAN_POINT('Ctrl Pts',(-2.37878753818289,291.411425943689,9.0087767276991));
#10618=CARTESIAN_POINT('Ctrl Pts',(-4.47163317015233,291.548925943689,7.81060623090856));
#10619=CARTESIAN_POINT('Ctrl Pts',(-6.56447880212178,291.686425943689,6.61243573411802));
#10620=CARTESIAN_POINT('Ctrl Pts',(-7.77785103721135,291.823925943689,4.52836682984767));
#10621=CARTESIAN_POINT('Ctrl Pts',(-8.99122327230091,291.961425943689,2.44429792557732));
#10622=CARTESIAN_POINT('Ctrl Pts',(-9.,292.098925943689,0.0327551936972079));
#10623=CARTESIAN_POINT('Ctrl Pts',(-9.0087767276991,292.236425943689,-2.3787875381829));
#10624=CARTESIAN_POINT('Ctrl Pts',(-7.81060623090856,292.373925943689,-4.47163317015234));
#10625=CARTESIAN_POINT('Ctrl Pts',(-6.61243573411802,292.511425943689,-6.56447880212179));
#10626=CARTESIAN_POINT('Ctrl Pts',(-4.52836682984766,292.648925943689,-7.77785103721135));
#10627=CARTESIAN_POINT('Ctrl Pts',(-2.44429792557731,292.786425943689,-8.99122327230091));
#10628=CARTESIAN_POINT('Ctrl Pts',(-0.0327551936972084,292.923925943689,
-9.));
#10629=CARTESIAN_POINT('Ctrl Pts',(2.3787875381829,293.061425943689,-9.0087767276991));
#10630=CARTESIAN_POINT('Ctrl Pts',(4.47163317015234,293.198925943689,-7.81060623090856));
#10631=CARTESIAN_POINT('Ctrl Pts',(6.56447880212178,293.336425943689,-6.61243573411802));
#10632=CARTESIAN_POINT('Ctrl Pts',(7.77785103721135,293.473925943689,-4.52836682984767));
#10633=CARTESIAN_POINT('Ctrl Pts',(8.99122327230091,293.611425943689,-2.44429792557732));
#10634=CARTESIAN_POINT('Ctrl Pts',(9.,293.748925943689,-0.032755193697209));
#10635=CARTESIAN_POINT('Ctrl Pts',(9.0087767276991,293.886425943689,2.37878753818289));
#10636=CARTESIAN_POINT('Ctrl Pts',(7.81060623090856,294.023925943689,4.47163317015234));
#10637=CARTESIAN_POINT('Ctrl Pts',(6.61243573411802,294.161425943689,6.56447880212178));
#10638=CARTESIAN_POINT('Ctrl Pts',(4.52836682984767,294.298925943689,7.77785103721135));
#10639=CARTESIAN_POINT('Ctrl Pts',(2.44429792557732,294.436425943689,8.99122327230091));
#10640=CARTESIAN_POINT('Ctrl Pts',(0.0327551936972095,294.573925943689,
9.));
#10641=CARTESIAN_POINT('Ctrl Pts',(-2.37878753818289,294.711425943689,9.0087767276991));
#10642=CARTESIAN_POINT('Ctrl Pts',(-4.47163317015233,294.848925943689,7.81060623090856));
#10643=CARTESIAN_POINT('Ctrl Pts',(-6.56447880212178,294.986425943689,6.61243573411802));
#10644=CARTESIAN_POINT('Ctrl Pts',(-7.77785103721135,295.123925943689,4.52836682984767));
#10645=CARTESIAN_POINT('Ctrl Pts',(-8.99122327230091,295.261425943689,2.44429792557732));
#10646=CARTESIAN_POINT('Ctrl Pts',(-9.,295.398925943689,0.0327551936972079));
#10647=CARTESIAN_POINT('Ctrl Pts',(-9.0087767276991,295.536425943689,-2.3787875381829));
#10648=CARTESIAN_POINT('Ctrl Pts',(-7.81060623090856,295.673925943689,-4.47163317015234));
#10649=CARTESIAN_POINT('Ctrl Pts',(-6.61243573411802,295.811425943689,-6.56447880212179));
#10650=CARTESIAN_POINT('Ctrl Pts',(-4.52836682984766,295.948925943689,-7.77785103721135));
#10651=CARTESIAN_POINT('Ctrl Pts',(-2.44429792557731,296.086425943689,-8.99122327230091));
#10652=CARTESIAN_POINT('Ctrl Pts',(-0.0327551936972084,296.223925943689,
-9.));
#10653=CARTESIAN_POINT('Ctrl Pts',(2.3787875381829,296.361425943689,-9.0087767276991));
#10654=CARTESIAN_POINT('Ctrl Pts',(4.47163317015234,296.498925943689,-7.81060623090856));
#10655=CARTESIAN_POINT('Ctrl Pts',(6.56447880212178,296.636425943689,-6.61243573411802));
#10656=CARTESIAN_POINT('Ctrl Pts',(7.77785103721135,296.773925943689,-4.52836682984767));
#10657=CARTESIAN_POINT('Ctrl Pts',(8.99122327230091,296.911425943689,-2.44429792557732));
#10658=CARTESIAN_POINT('Ctrl Pts',(9.,297.048925943689,-0.032755193697209));
#10659=CARTESIAN_POINT('Ctrl Pts',(9.0087767276991,297.186425943689,2.37878753818289));
#10660=CARTESIAN_POINT('Ctrl Pts',(7.81060623090856,297.323925943689,4.47163317015234));
#10661=CARTESIAN_POINT('Ctrl Pts',(6.61243573411802,297.461425943689,6.56447880212178));
#10662=CARTESIAN_POINT('Ctrl Pts',(4.52836682984767,297.598925943689,7.77785103721135));
#10663=CARTESIAN_POINT('Ctrl Pts',(2.44429792557732,297.736425943689,8.99122327230091));
#10664=CARTESIAN_POINT('Ctrl Pts',(0.0327551936972095,297.873925943689,
9.));
#10665=CARTESIAN_POINT('Ctrl Pts',(-2.37878753818289,298.011425943689,9.0087767276991));
#10666=CARTESIAN_POINT('Ctrl Pts',(-4.47163317015233,298.148925943689,7.81060623090856));
#10667=CARTESIAN_POINT('Ctrl Pts',(-6.56447880212178,298.286425943689,6.61243573411802));
#10668=CARTESIAN_POINT('Ctrl Pts',(-7.77785103721135,298.423925943689,4.52836682984767));
#10669=CARTESIAN_POINT('Ctrl Pts',(-8.99122327230091,298.561425943689,2.44429792557732));
#10670=CARTESIAN_POINT('Ctrl Pts',(-9.,298.698925943689,0.0327551936972079));
#10671=CARTESIAN_POINT('Ctrl Pts',(-9.0087767276991,298.836425943689,-2.3787875381829));
#10672=CARTESIAN_POINT('Ctrl Pts',(-7.81060623090856,298.973925943689,-4.47163317015234));
#10673=CARTESIAN_POINT('Ctrl Pts',(-6.61243573411802,299.111425943689,-6.56447880212179));
#10674=CARTESIAN_POINT('Ctrl Pts',(-4.52836682984766,299.248925943689,-7.77785103721135));
#10675=CARTESIAN_POINT('Ctrl Pts',(-2.44429792557731,299.386425943689,-8.99122327230091));
#10676=CARTESIAN_POINT('Ctrl Pts',(-0.0327551936972084,299.523925943689,
-9.));
#10677=CARTESIAN_POINT('Ctrl Pts',(2.3787875381829,299.661425943689,-9.0087767276991));
#10678=CARTESIAN_POINT('Ctrl Pts',(4.47163317015234,299.798925943689,-7.81060623090856));
#10679=CARTESIAN_POINT('Ctrl Pts',(6.56447880212178,299.936425943689,-6.61243573411802));
#10680=CARTESIAN_POINT('Ctrl Pts',(7.77785103721135,300.073925943689,-4.52836682984767));
#10681=CARTESIAN_POINT('Ctrl Pts',(8.99122327230091,300.211425943689,-2.44429792557732));
#10682=CARTESIAN_POINT('Ctrl Pts',(9.,300.348925943689,-0.032755193697209));
#10683=CARTESIAN_POINT('Ctrl Pts',(9.0087767276991,300.486425943689,2.37878753818289));
#10684=CARTESIAN_POINT('Ctrl Pts',(7.81060623090856,300.623925943689,4.47163317015234));
#10685=CARTESIAN_POINT('Ctrl Pts',(6.61243573411802,300.761425943689,6.56447880212178));
#10686=CARTESIAN_POINT('Ctrl Pts',(4.52836682984767,300.898925943689,7.77785103721135));
#10687=CARTESIAN_POINT('Ctrl Pts',(2.44429792557732,301.036425943689,8.99122327230091));
#10688=CARTESIAN_POINT('Ctrl Pts',(0.0327551936972095,301.173925943689,
9.));
#10689=CARTESIAN_POINT('Ctrl Pts',(-2.37878753818289,301.311425943689,9.0087767276991));
#10690=CARTESIAN_POINT('Ctrl Pts',(-4.47163317015233,301.448925943689,7.81060623090856));
#10691=CARTESIAN_POINT('Ctrl Pts',(-6.56447880212178,301.586425943689,6.61243573411802));
#10692=CARTESIAN_POINT('Ctrl Pts',(-7.77785103721135,301.723925943689,4.52836682984767));
#10693=CARTESIAN_POINT('Ctrl Pts',(-8.99122327230091,301.861425943689,2.44429792557732));
#10694=CARTESIAN_POINT('Ctrl Pts',(-9.,301.998925943689,0.0327551936972079));
#10695=CARTESIAN_POINT('Ctrl Pts',(-9.0087767276991,302.136425943689,-2.3787875381829));
#10696=CARTESIAN_POINT('Ctrl Pts',(-7.81060623090856,302.273925943689,-4.47163317015234));
#10697=CARTESIAN_POINT('Ctrl Pts',(-6.61243573411802,302.411425943689,-6.56447880212179));
#10698=CARTESIAN_POINT('Ctrl Pts',(-4.52836682984766,302.548925943689,-7.77785103721135));
#10699=CARTESIAN_POINT('Ctrl Pts',(-2.44429792557731,302.686425943689,-8.99122327230091));
#10700=CARTESIAN_POINT('Ctrl Pts',(-0.0327551936972084,302.823925943689,
-9.));
#10701=CARTESIAN_POINT('Ctrl Pts',(2.3787875381829,302.961425943689,-9.0087767276991));
#10702=CARTESIAN_POINT('Ctrl Pts',(4.47163317015234,303.098925943689,-7.81060623090856));
#10703=CARTESIAN_POINT('Ctrl Pts',(6.56447880212178,303.236425943689,-6.61243573411802));
#10704=CARTESIAN_POINT('Ctrl Pts',(7.77785103721135,303.373925943689,-4.52836682984767));
#10705=CARTESIAN_POINT('Ctrl Pts',(8.99122327230091,303.511425943689,-2.44429792557732));
#10706=CARTESIAN_POINT('Ctrl Pts',(9.,303.648925943689,-0.032755193697209));
#10707=CARTESIAN_POINT('Ctrl Pts',(9.0087767276991,303.786425943689,2.37878753818289));
#10708=CARTESIAN_POINT('Ctrl Pts',(7.81060623090856,303.923925943689,4.47163317015234));
#10709=CARTESIAN_POINT('Ctrl Pts',(6.61243573411802,304.061425943689,6.56447880212178));
#10710=CARTESIAN_POINT('Ctrl Pts',(4.52836682984767,304.198925943689,7.77785103721135));
#10711=CARTESIAN_POINT('Ctrl Pts',(2.44429792557732,304.336425943689,8.99122327230091));
#10712=CARTESIAN_POINT('Ctrl Pts',(0.0327551936972095,304.473925943689,
9.));
#10713=CARTESIAN_POINT('Ctrl Pts',(-2.37878753818289,304.611425943689,9.0087767276991));
#10714=CARTESIAN_POINT('Ctrl Pts',(-4.47163317015233,304.748925943689,7.81060623090856));
#10715=CARTESIAN_POINT('Ctrl Pts',(-6.56447880212178,304.886425943689,6.61243573411802));
#10716=CARTESIAN_POINT('Ctrl Pts',(-7.77785103721135,305.023925943689,4.52836682984767));
#10717=CARTESIAN_POINT('Ctrl Pts',(-8.99122327230091,305.161425943689,2.44429792557732));
#10718=CARTESIAN_POINT('Ctrl Pts',(-9.,305.298925943689,0.0327551936972079));
#10719=CARTESIAN_POINT('Ctrl Pts',(-9.0087767276991,305.436425943689,-2.3787875381829));
#10720=CARTESIAN_POINT('Ctrl Pts',(-7.81060623090856,305.573925943689,-4.47163317015234));
#10721=CARTESIAN_POINT('Ctrl Pts',(-6.61243573411802,305.711425943689,-6.56447880212179));
#10722=CARTESIAN_POINT('Ctrl Pts',(-4.52836682984766,305.848925943689,-7.77785103721135));
#10723=CARTESIAN_POINT('Ctrl Pts',(-2.44429792557731,305.986425943689,-8.99122327230091));
#10724=CARTESIAN_POINT('Ctrl Pts',(-0.0327551936972084,306.123925943689,
-9.));
#10725=CARTESIAN_POINT('Ctrl Pts',(2.3787875381829,306.261425943689,-9.0087767276991));
#10726=CARTESIAN_POINT('Ctrl Pts',(4.47163317015234,306.398925943689,-7.81060623090856));
#10727=CARTESIAN_POINT('Ctrl Pts',(6.56447880212178,306.536425943689,-6.61243573411802));
#10728=CARTESIAN_POINT('Ctrl Pts',(7.77785103721135,306.673925943689,-4.52836682984767));
#10729=CARTESIAN_POINT('Ctrl Pts',(8.99122327230091,306.811425943689,-2.44429792557732));
#10730=CARTESIAN_POINT('Ctrl Pts',(9.,306.948925943689,-0.032755193697209));
#10731=CARTESIAN_POINT('Ctrl Pts',(9.0087767276991,307.086425943689,2.37878753818289));
#10732=CARTESIAN_POINT('Ctrl Pts',(7.81060623090856,307.223925943689,4.47163317015234));
#10733=CARTESIAN_POINT('Ctrl Pts',(6.61243573411802,307.361425943689,6.56447880212178));
#10734=CARTESIAN_POINT('Ctrl Pts',(4.52836682984767,307.498925943689,7.77785103721135));
#10735=CARTESIAN_POINT('Ctrl Pts',(2.44429792557732,307.636425943689,8.99122327230091));
#10736=CARTESIAN_POINT('Ctrl Pts',(0.0327551936972095,307.773925943689,
9.));
#10737=CARTESIAN_POINT('Ctrl Pts',(-2.37878753818289,307.911425943689,9.0087767276991));
#10738=CARTESIAN_POINT('Ctrl Pts',(-4.47163317015233,308.048925943689,7.81060623090856));
#10739=CARTESIAN_POINT('Ctrl Pts',(-6.56447880212178,308.186425943689,6.61243573411802));
#10740=CARTESIAN_POINT('Ctrl Pts',(-7.77785103721135,308.323925943689,4.52836682984767));
#10741=CARTESIAN_POINT('Ctrl Pts',(-8.99122327230091,308.461425943689,2.44429792557732));
#10742=CARTESIAN_POINT('Ctrl Pts',(-9.,308.598925943689,0.0327551936972079));
#10743=CARTESIAN_POINT('Ctrl Pts',(-9.0087767276991,308.736425943689,-2.3787875381829));
#10744=CARTESIAN_POINT('Ctrl Pts',(-7.81060623090856,308.873925943689,-4.47163317015234));
#10745=CARTESIAN_POINT('Ctrl Pts',(-6.61243573411802,309.011425943689,-6.56447880212179));
#10746=CARTESIAN_POINT('Ctrl Pts',(-4.52836682984766,309.148925943689,-7.77785103721135));
#10747=CARTESIAN_POINT('Ctrl Pts',(-2.44429792557731,309.286425943689,-8.99122327230091));
#10748=CARTESIAN_POINT('Ctrl Pts',(-0.0327551936972084,309.423925943689,
-9.));
#10749=CARTESIAN_POINT('Ctrl Pts',(2.3787875381829,309.561425943689,-9.0087767276991));
#10750=CARTESIAN_POINT('Ctrl Pts',(4.47163317015234,309.698925943689,-7.81060623090856));
#10751=CARTESIAN_POINT('Ctrl Pts',(6.56447880212178,309.836425943689,-6.61243573411802));
#10752=CARTESIAN_POINT('Ctrl Pts',(7.77785103721135,309.973925943689,-4.52836682984767));
#10753=CARTESIAN_POINT('Ctrl Pts',(8.99122327230091,310.111425943689,-2.44429792557732));
#10754=CARTESIAN_POINT('Ctrl Pts',(9.,310.248925943689,-0.032755193697209));
#10755=CARTESIAN_POINT('Ctrl Pts',(9.0087767276991,310.386425943689,2.37878753818289));
#10756=CARTESIAN_POINT('Ctrl Pts',(7.81060623090856,310.523925943689,4.47163317015234));
#10757=CARTESIAN_POINT('Ctrl Pts',(6.61243573411802,310.661425943689,6.56447880212178));
#10758=CARTESIAN_POINT('Ctrl Pts',(4.52836682984767,310.798925943689,7.77785103721135));
#10759=CARTESIAN_POINT('Ctrl Pts',(2.44429792557732,310.936425943689,8.99122327230091));
#10760=CARTESIAN_POINT('Ctrl Pts',(0.0327551936972095,311.073925943689,
9.));
#10761=CARTESIAN_POINT('Ctrl Pts',(-2.37878753818289,311.211425943689,9.0087767276991));
#10762=CARTESIAN_POINT('Ctrl Pts',(-4.47163317015233,311.348925943689,7.81060623090856));
#10763=CARTESIAN_POINT('Ctrl Pts',(-6.56447880212178,311.486425943689,6.61243573411802));
#10764=CARTESIAN_POINT('Ctrl Pts',(-7.77785103721135,311.623925943689,4.52836682984767));
#10765=CARTESIAN_POINT('Ctrl Pts',(-8.99122327230091,311.761425943689,2.44429792557732));
#10766=CARTESIAN_POINT('Ctrl Pts',(-9.,311.898925943689,0.0327551936972079));
#10767=CARTESIAN_POINT('Ctrl Pts',(-9.0087767276991,312.036425943689,-2.3787875381829));
#10768=CARTESIAN_POINT('Ctrl Pts',(-7.81060623090856,312.173925943689,-4.47163317015234));
#10769=CARTESIAN_POINT('Ctrl Pts',(-6.61243573411802,312.311425943689,-6.56447880212179));
#10770=CARTESIAN_POINT('Ctrl Pts',(-4.52836682984766,312.448925943689,-7.77785103721135));
#10771=CARTESIAN_POINT('Ctrl Pts',(-2.44429792557731,312.586425943689,-8.99122327230091));
#10772=CARTESIAN_POINT('Ctrl Pts',(-0.0327551936972084,312.723925943689,
-9.));
#10773=CARTESIAN_POINT('Ctrl Pts',(2.3787875381829,312.861425943689,-9.0087767276991));
#10774=CARTESIAN_POINT('Ctrl Pts',(4.47163317015234,312.998925943689,-7.81060623090856));
#10775=CARTESIAN_POINT('Ctrl Pts',(6.56447880212178,313.136425943689,-6.61243573411802));
#10776=CARTESIAN_POINT('Ctrl Pts',(7.77785103721135,313.273925943689,-4.52836682984767));
#10777=CARTESIAN_POINT('Ctrl Pts',(8.99122327230091,313.411425943689,-2.44429792557732));
#10778=CARTESIAN_POINT('Ctrl Pts',(9.,313.548925943689,-0.032755193697209));
#10779=CARTESIAN_POINT('Ctrl Pts',(9.0087767276991,313.686425943689,2.37878753818289));
#10780=CARTESIAN_POINT('Ctrl Pts',(7.81060623090856,313.823925943689,4.47163317015234));
#10781=CARTESIAN_POINT('Ctrl Pts',(6.61243573411802,313.961425943689,6.56447880212178));
#10782=CARTESIAN_POINT('Ctrl Pts',(4.52836682984767,314.098925943689,7.77785103721135));
#10783=CARTESIAN_POINT('Ctrl Pts',(2.44429792557732,314.236425943689,8.99122327230091));
#10784=CARTESIAN_POINT('Ctrl Pts',(0.0327551936972095,314.373925943689,
9.));
#10785=CARTESIAN_POINT('Ctrl Pts',(-2.37878753818289,314.511425943689,9.0087767276991));
#10786=CARTESIAN_POINT('Ctrl Pts',(-4.47163317015233,314.648925943689,7.81060623090856));
#10787=CARTESIAN_POINT('Ctrl Pts',(-6.56447880212178,314.786425943689,6.61243573411802));
#10788=CARTESIAN_POINT('Ctrl Pts',(-7.77785103721135,314.923925943689,4.52836682984767));
#10789=CARTESIAN_POINT('Ctrl Pts',(-8.99122327230091,315.061425943689,2.44429792557732));
#10790=CARTESIAN_POINT('Ctrl Pts',(-9.,315.198925943689,0.0327551936972079));
#10791=CARTESIAN_POINT('Ctrl Pts',(-9.0087767276991,315.336425943689,-2.3787875381829));
#10792=CARTESIAN_POINT('Ctrl Pts',(-7.81060623090856,315.473925943689,-4.47163317015234));
#10793=CARTESIAN_POINT('Ctrl Pts',(-6.61243573411802,315.611425943689,-6.56447880212179));
#10794=CARTESIAN_POINT('Ctrl Pts',(-4.52836682984766,315.748925943689,-7.77785103721135));
#10795=CARTESIAN_POINT('Ctrl Pts',(-2.44429792557731,315.886425943689,-8.99122327230091));
#10796=CARTESIAN_POINT('Ctrl Pts',(-0.0327551936972084,316.023925943689,
-9.));
#10797=CARTESIAN_POINT('Ctrl Pts',(2.3787875381829,316.161425943689,-9.0087767276991));
#10798=CARTESIAN_POINT('Ctrl Pts',(4.47163317015234,316.298925943689,-7.81060623090856));
#10799=CARTESIAN_POINT('Ctrl Pts',(6.56447880212178,316.436425943689,-6.61243573411802));
#10800=CARTESIAN_POINT('Ctrl Pts',(7.77785103721135,316.573925943689,-4.52836682984767));
#10801=CARTESIAN_POINT('Ctrl Pts',(8.99122327230091,316.711425943689,-2.44429792557732));
#10802=CARTESIAN_POINT('Ctrl Pts',(9.,316.848925943689,-0.032755193697209));
#10803=CARTESIAN_POINT('Ctrl Pts',(9.0087767276991,316.986425943689,2.37878753818289));
#10804=CARTESIAN_POINT('Ctrl Pts',(7.81060623090856,317.123925943689,4.47163317015234));
#10805=CARTESIAN_POINT('Ctrl Pts',(6.61243573411802,317.261425943689,6.56447880212178));
#10806=CARTESIAN_POINT('Ctrl Pts',(4.52836682984767,317.398925943689,7.77785103721135));
#10807=CARTESIAN_POINT('Ctrl Pts',(2.44429792557732,317.536425943689,8.99122327230091));
#10808=CARTESIAN_POINT('Ctrl Pts',(0.0327551936972095,317.673925943689,
9.));
#10809=CARTESIAN_POINT('Ctrl Pts',(-2.37878753818289,317.811425943689,9.0087767276991));
#10810=CARTESIAN_POINT('Ctrl Pts',(-4.47163317015233,317.948925943689,7.81060623090856));
#10811=CARTESIAN_POINT('Ctrl Pts',(-6.56447880212178,318.086425943689,6.61243573411802));
#10812=CARTESIAN_POINT('Ctrl Pts',(-7.77785103721135,318.223925943689,4.52836682984767));
#10813=CARTESIAN_POINT('Ctrl Pts',(-8.99122327230091,318.361425943689,2.44429792557732));
#10814=CARTESIAN_POINT('Ctrl Pts',(-9.,318.498925943689,0.0327551936972079));
#10815=CARTESIAN_POINT('Ctrl Pts',(-8.,285.498925943689,0.0327551936971979));
#10816=CARTESIAN_POINT('Ctrl Pts',(-8.00877672769909,285.636425943689,-2.11083834575178));
#10817=CARTESIAN_POINT('Ctrl Pts',(-6.94458082712411,285.773925943689,-3.97163317015235));
#10818=CARTESIAN_POINT('Ctrl Pts',(-5.88038492654913,285.911425943689,-5.83242799455291));
#10819=CARTESIAN_POINT('Ctrl Pts',(-4.02836682984766,286.048925943689,-6.91182563342691));
#10820=CARTESIAN_POINT('Ctrl Pts',(-2.17634873314618,286.186425943689,-7.99122327230091));
#10821=CARTESIAN_POINT('Ctrl Pts',(-0.0327551936971984,286.323925943689,
-8.));
#10822=CARTESIAN_POINT('Ctrl Pts',(2.11083834575178,286.461425943689,-8.00877672769909));
#10823=CARTESIAN_POINT('Ctrl Pts',(3.97163317015235,286.598925943689,-6.94458082712411));
#10824=CARTESIAN_POINT('Ctrl Pts',(5.83242799455291,286.736425943689,-5.88038492654913));
#10825=CARTESIAN_POINT('Ctrl Pts',(6.91182563342691,286.873925943689,-4.02836682984766));
#10826=CARTESIAN_POINT('Ctrl Pts',(7.99122327230091,287.011425943689,-2.17634873314618));
#10827=CARTESIAN_POINT('Ctrl Pts',(8.,287.148925943689,-0.0327551936971989));
#10828=CARTESIAN_POINT('Ctrl Pts',(8.00877672769909,287.286425943689,2.11083834575178));
#10829=CARTESIAN_POINT('Ctrl Pts',(6.94458082712411,287.423925943689,3.97163317015235));
#10830=CARTESIAN_POINT('Ctrl Pts',(5.88038492654913,287.561425943689,5.83242799455291));
#10831=CARTESIAN_POINT('Ctrl Pts',(4.02836682984766,287.698925943689,6.91182563342691));
#10832=CARTESIAN_POINT('Ctrl Pts',(2.17634873314619,287.836425943689,7.99122327230091));
#10833=CARTESIAN_POINT('Ctrl Pts',(0.0327551936971994,287.973925943689,
8.));
#10834=CARTESIAN_POINT('Ctrl Pts',(-2.11083834575178,288.111425943689,8.00877672769909));
#10835=CARTESIAN_POINT('Ctrl Pts',(-3.97163317015234,288.248925943689,6.94458082712412));
#10836=CARTESIAN_POINT('Ctrl Pts',(-5.83242799455291,288.386425943689,5.88038492654913));
#10837=CARTESIAN_POINT('Ctrl Pts',(-6.91182563342691,288.523925943689,4.02836682984766));
#10838=CARTESIAN_POINT('Ctrl Pts',(-7.99122327230091,288.661425943689,2.17634873314619));
#10839=CARTESIAN_POINT('Ctrl Pts',(-8.,288.798925943689,0.0327551936971979));
#10840=CARTESIAN_POINT('Ctrl Pts',(-8.00877672769909,288.936425943689,-2.11083834575178));
#10841=CARTESIAN_POINT('Ctrl Pts',(-6.94458082712411,289.073925943689,-3.97163317015235));
#10842=CARTESIAN_POINT('Ctrl Pts',(-5.88038492654913,289.211425943689,-5.83242799455291));
#10843=CARTESIAN_POINT('Ctrl Pts',(-4.02836682984766,289.348925943689,-6.91182563342691));
#10844=CARTESIAN_POINT('Ctrl Pts',(-2.17634873314618,289.486425943689,-7.99122327230091));
#10845=CARTESIAN_POINT('Ctrl Pts',(-0.0327551936971984,289.623925943689,
-8.));
#10846=CARTESIAN_POINT('Ctrl Pts',(2.11083834575178,289.761425943689,-8.00877672769909));
#10847=CARTESIAN_POINT('Ctrl Pts',(3.97163317015235,289.898925943689,-6.94458082712411));
#10848=CARTESIAN_POINT('Ctrl Pts',(5.83242799455291,290.036425943689,-5.88038492654913));
#10849=CARTESIAN_POINT('Ctrl Pts',(6.91182563342691,290.173925943689,-4.02836682984766));
#10850=CARTESIAN_POINT('Ctrl Pts',(7.99122327230091,290.311425943689,-2.17634873314618));
#10851=CARTESIAN_POINT('Ctrl Pts',(8.,290.448925943689,-0.0327551936971989));
#10852=CARTESIAN_POINT('Ctrl Pts',(8.00877672769909,290.586425943689,2.11083834575178));
#10853=CARTESIAN_POINT('Ctrl Pts',(6.94458082712411,290.723925943689,3.97163317015235));
#10854=CARTESIAN_POINT('Ctrl Pts',(5.88038492654913,290.861425943689,5.83242799455291));
#10855=CARTESIAN_POINT('Ctrl Pts',(4.02836682984766,290.998925943689,6.91182563342691));
#10856=CARTESIAN_POINT('Ctrl Pts',(2.17634873314619,291.136425943689,7.99122327230091));
#10857=CARTESIAN_POINT('Ctrl Pts',(0.0327551936971994,291.273925943689,
8.));
#10858=CARTESIAN_POINT('Ctrl Pts',(-2.11083834575178,291.411425943689,8.00877672769909));
#10859=CARTESIAN_POINT('Ctrl Pts',(-3.97163317015234,291.548925943689,6.94458082712412));
#10860=CARTESIAN_POINT('Ctrl Pts',(-5.83242799455291,291.686425943689,5.88038492654913));
#10861=CARTESIAN_POINT('Ctrl Pts',(-6.91182563342691,291.823925943689,4.02836682984766));
#10862=CARTESIAN_POINT('Ctrl Pts',(-7.99122327230091,291.961425943689,2.17634873314619));
#10863=CARTESIAN_POINT('Ctrl Pts',(-8.,292.098925943689,0.0327551936971979));
#10864=CARTESIAN_POINT('Ctrl Pts',(-8.00877672769909,292.236425943689,-2.11083834575178));
#10865=CARTESIAN_POINT('Ctrl Pts',(-6.94458082712411,292.373925943689,-3.97163317015235));
#10866=CARTESIAN_POINT('Ctrl Pts',(-5.88038492654913,292.511425943689,-5.83242799455291));
#10867=CARTESIAN_POINT('Ctrl Pts',(-4.02836682984766,292.648925943689,-6.91182563342691));
#10868=CARTESIAN_POINT('Ctrl Pts',(-2.17634873314618,292.786425943689,-7.99122327230091));
#10869=CARTESIAN_POINT('Ctrl Pts',(-0.0327551936971984,292.923925943689,
-8.));
#10870=CARTESIAN_POINT('Ctrl Pts',(2.11083834575178,293.061425943689,-8.00877672769909));
#10871=CARTESIAN_POINT('Ctrl Pts',(3.97163317015235,293.198925943689,-6.94458082712411));
#10872=CARTESIAN_POINT('Ctrl Pts',(5.83242799455291,293.336425943689,-5.88038492654913));
#10873=CARTESIAN_POINT('Ctrl Pts',(6.91182563342691,293.473925943689,-4.02836682984766));
#10874=CARTESIAN_POINT('Ctrl Pts',(7.99122327230091,293.611425943689,-2.17634873314618));
#10875=CARTESIAN_POINT('Ctrl Pts',(8.,293.748925943689,-0.0327551936971989));
#10876=CARTESIAN_POINT('Ctrl Pts',(8.00877672769909,293.886425943689,2.11083834575178));
#10877=CARTESIAN_POINT('Ctrl Pts',(6.94458082712411,294.023925943689,3.97163317015235));
#10878=CARTESIAN_POINT('Ctrl Pts',(5.88038492654913,294.161425943689,5.83242799455291));
#10879=CARTESIAN_POINT('Ctrl Pts',(4.02836682984766,294.298925943689,6.91182563342691));
#10880=CARTESIAN_POINT('Ctrl Pts',(2.17634873314619,294.436425943689,7.99122327230091));
#10881=CARTESIAN_POINT('Ctrl Pts',(0.0327551936971994,294.573925943689,
8.));
#10882=CARTESIAN_POINT('Ctrl Pts',(-2.11083834575178,294.711425943689,8.00877672769909));
#10883=CARTESIAN_POINT('Ctrl Pts',(-3.97163317015234,294.848925943689,6.94458082712412));
#10884=CARTESIAN_POINT('Ctrl Pts',(-5.83242799455291,294.986425943689,5.88038492654913));
#10885=CARTESIAN_POINT('Ctrl Pts',(-6.91182563342691,295.123925943689,4.02836682984766));
#10886=CARTESIAN_POINT('Ctrl Pts',(-7.99122327230091,295.261425943689,2.17634873314619));
#10887=CARTESIAN_POINT('Ctrl Pts',(-8.,295.398925943689,0.0327551936971979));
#10888=CARTESIAN_POINT('Ctrl Pts',(-8.00877672769909,295.536425943689,-2.11083834575178));
#10889=CARTESIAN_POINT('Ctrl Pts',(-6.94458082712411,295.673925943689,-3.97163317015235));
#10890=CARTESIAN_POINT('Ctrl Pts',(-5.88038492654913,295.811425943689,-5.83242799455291));
#10891=CARTESIAN_POINT('Ctrl Pts',(-4.02836682984766,295.948925943689,-6.91182563342691));
#10892=CARTESIAN_POINT('Ctrl Pts',(-2.17634873314618,296.086425943689,-7.99122327230091));
#10893=CARTESIAN_POINT('Ctrl Pts',(-0.0327551936971984,296.223925943689,
-8.));
#10894=CARTESIAN_POINT('Ctrl Pts',(2.11083834575178,296.361425943689,-8.00877672769909));
#10895=CARTESIAN_POINT('Ctrl Pts',(3.97163317015235,296.498925943689,-6.94458082712411));
#10896=CARTESIAN_POINT('Ctrl Pts',(5.83242799455291,296.636425943689,-5.88038492654913));
#10897=CARTESIAN_POINT('Ctrl Pts',(6.91182563342691,296.773925943689,-4.02836682984766));
#10898=CARTESIAN_POINT('Ctrl Pts',(7.99122327230091,296.911425943689,-2.17634873314618));
#10899=CARTESIAN_POINT('Ctrl Pts',(8.,297.048925943689,-0.0327551936971989));
#10900=CARTESIAN_POINT('Ctrl Pts',(8.00877672769909,297.186425943689,2.11083834575178));
#10901=CARTESIAN_POINT('Ctrl Pts',(6.94458082712411,297.323925943689,3.97163317015235));
#10902=CARTESIAN_POINT('Ctrl Pts',(5.88038492654913,297.461425943689,5.83242799455291));
#10903=CARTESIAN_POINT('Ctrl Pts',(4.02836682984766,297.598925943689,6.91182563342691));
#10904=CARTESIAN_POINT('Ctrl Pts',(2.17634873314619,297.736425943689,7.99122327230091));
#10905=CARTESIAN_POINT('Ctrl Pts',(0.0327551936971994,297.873925943689,
8.));
#10906=CARTESIAN_POINT('Ctrl Pts',(-2.11083834575178,298.011425943689,8.00877672769909));
#10907=CARTESIAN_POINT('Ctrl Pts',(-3.97163317015234,298.148925943689,6.94458082712412));
#10908=CARTESIAN_POINT('Ctrl Pts',(-5.83242799455291,298.286425943689,5.88038492654913));
#10909=CARTESIAN_POINT('Ctrl Pts',(-6.91182563342691,298.423925943689,4.02836682984766));
#10910=CARTESIAN_POINT('Ctrl Pts',(-7.99122327230091,298.561425943689,2.17634873314619));
#10911=CARTESIAN_POINT('Ctrl Pts',(-8.,298.698925943689,0.0327551936971979));
#10912=CARTESIAN_POINT('Ctrl Pts',(-8.00877672769909,298.836425943689,-2.11083834575178));
#10913=CARTESIAN_POINT('Ctrl Pts',(-6.94458082712411,298.973925943689,-3.97163317015235));
#10914=CARTESIAN_POINT('Ctrl Pts',(-5.88038492654913,299.111425943689,-5.83242799455291));
#10915=CARTESIAN_POINT('Ctrl Pts',(-4.02836682984766,299.248925943689,-6.91182563342691));
#10916=CARTESIAN_POINT('Ctrl Pts',(-2.17634873314618,299.386425943689,-7.99122327230091));
#10917=CARTESIAN_POINT('Ctrl Pts',(-0.0327551936971984,299.523925943689,
-8.));
#10918=CARTESIAN_POINT('Ctrl Pts',(2.11083834575178,299.661425943689,-8.00877672769909));
#10919=CARTESIAN_POINT('Ctrl Pts',(3.97163317015235,299.798925943689,-6.94458082712411));
#10920=CARTESIAN_POINT('Ctrl Pts',(5.83242799455291,299.936425943689,-5.88038492654913));
#10921=CARTESIAN_POINT('Ctrl Pts',(6.91182563342691,300.073925943689,-4.02836682984766));
#10922=CARTESIAN_POINT('Ctrl Pts',(7.99122327230091,300.211425943689,-2.17634873314618));
#10923=CARTESIAN_POINT('Ctrl Pts',(8.,300.348925943689,-0.0327551936971989));
#10924=CARTESIAN_POINT('Ctrl Pts',(8.00877672769909,300.486425943689,2.11083834575178));
#10925=CARTESIAN_POINT('Ctrl Pts',(6.94458082712411,300.623925943689,3.97163317015235));
#10926=CARTESIAN_POINT('Ctrl Pts',(5.88038492654913,300.761425943689,5.83242799455291));
#10927=CARTESIAN_POINT('Ctrl Pts',(4.02836682984766,300.898925943689,6.91182563342691));
#10928=CARTESIAN_POINT('Ctrl Pts',(2.17634873314619,301.036425943689,7.99122327230091));
#10929=CARTESIAN_POINT('Ctrl Pts',(0.0327551936971994,301.173925943689,
8.));
#10930=CARTESIAN_POINT('Ctrl Pts',(-2.11083834575178,301.311425943689,8.00877672769909));
#10931=CARTESIAN_POINT('Ctrl Pts',(-3.97163317015234,301.448925943689,6.94458082712412));
#10932=CARTESIAN_POINT('Ctrl Pts',(-5.83242799455291,301.586425943689,5.88038492654913));
#10933=CARTESIAN_POINT('Ctrl Pts',(-6.91182563342691,301.723925943689,4.02836682984766));
#10934=CARTESIAN_POINT('Ctrl Pts',(-7.99122327230091,301.861425943689,2.17634873314619));
#10935=CARTESIAN_POINT('Ctrl Pts',(-8.,301.998925943689,0.0327551936971979));
#10936=CARTESIAN_POINT('Ctrl Pts',(-8.00877672769909,302.136425943689,-2.11083834575178));
#10937=CARTESIAN_POINT('Ctrl Pts',(-6.94458082712411,302.273925943689,-3.97163317015235));
#10938=CARTESIAN_POINT('Ctrl Pts',(-5.88038492654913,302.411425943689,-5.83242799455291));
#10939=CARTESIAN_POINT('Ctrl Pts',(-4.02836682984766,302.548925943689,-6.91182563342691));
#10940=CARTESIAN_POINT('Ctrl Pts',(-2.17634873314618,302.686425943689,-7.99122327230091));
#10941=CARTESIAN_POINT('Ctrl Pts',(-0.0327551936971984,302.823925943689,
-8.));
#10942=CARTESIAN_POINT('Ctrl Pts',(2.11083834575178,302.961425943689,-8.00877672769909));
#10943=CARTESIAN_POINT('Ctrl Pts',(3.97163317015235,303.098925943689,-6.94458082712411));
#10944=CARTESIAN_POINT('Ctrl Pts',(5.83242799455291,303.236425943689,-5.88038492654913));
#10945=CARTESIAN_POINT('Ctrl Pts',(6.91182563342691,303.373925943689,-4.02836682984766));
#10946=CARTESIAN_POINT('Ctrl Pts',(7.99122327230091,303.511425943689,-2.17634873314618));
#10947=CARTESIAN_POINT('Ctrl Pts',(8.,303.648925943689,-0.0327551936971989));
#10948=CARTESIAN_POINT('Ctrl Pts',(8.00877672769909,303.786425943689,2.11083834575178));
#10949=CARTESIAN_POINT('Ctrl Pts',(6.94458082712411,303.923925943689,3.97163317015235));
#10950=CARTESIAN_POINT('Ctrl Pts',(5.88038492654913,304.061425943689,5.83242799455291));
#10951=CARTESIAN_POINT('Ctrl Pts',(4.02836682984766,304.198925943689,6.91182563342691));
#10952=CARTESIAN_POINT('Ctrl Pts',(2.17634873314619,304.336425943689,7.99122327230091));
#10953=CARTESIAN_POINT('Ctrl Pts',(0.0327551936971994,304.473925943689,
8.));
#10954=CARTESIAN_POINT('Ctrl Pts',(-2.11083834575178,304.611425943689,8.00877672769909));
#10955=CARTESIAN_POINT('Ctrl Pts',(-3.97163317015234,304.748925943689,6.94458082712412));
#10956=CARTESIAN_POINT('Ctrl Pts',(-5.83242799455291,304.886425943689,5.88038492654913));
#10957=CARTESIAN_POINT('Ctrl Pts',(-6.91182563342691,305.023925943689,4.02836682984766));
#10958=CARTESIAN_POINT('Ctrl Pts',(-7.99122327230091,305.161425943689,2.17634873314619));
#10959=CARTESIAN_POINT('Ctrl Pts',(-8.,305.298925943689,0.0327551936971979));
#10960=CARTESIAN_POINT('Ctrl Pts',(-8.00877672769909,305.436425943689,-2.11083834575178));
#10961=CARTESIAN_POINT('Ctrl Pts',(-6.94458082712411,305.573925943689,-3.97163317015235));
#10962=CARTESIAN_POINT('Ctrl Pts',(-5.88038492654913,305.711425943689,-5.83242799455291));
#10963=CARTESIAN_POINT('Ctrl Pts',(-4.02836682984766,305.848925943689,-6.91182563342691));
#10964=CARTESIAN_POINT('Ctrl Pts',(-2.17634873314618,305.986425943689,-7.99122327230091));
#10965=CARTESIAN_POINT('Ctrl Pts',(-0.0327551936971984,306.123925943689,
-8.));
#10966=CARTESIAN_POINT('Ctrl Pts',(2.11083834575178,306.261425943689,-8.00877672769909));
#10967=CARTESIAN_POINT('Ctrl Pts',(3.97163317015235,306.398925943689,-6.94458082712411));
#10968=CARTESIAN_POINT('Ctrl Pts',(5.83242799455291,306.536425943689,-5.88038492654913));
#10969=CARTESIAN_POINT('Ctrl Pts',(6.91182563342691,306.673925943689,-4.02836682984766));
#10970=CARTESIAN_POINT('Ctrl Pts',(7.99122327230091,306.811425943689,-2.17634873314618));
#10971=CARTESIAN_POINT('Ctrl Pts',(8.,306.948925943689,-0.0327551936971989));
#10972=CARTESIAN_POINT('Ctrl Pts',(8.00877672769909,307.086425943689,2.11083834575178));
#10973=CARTESIAN_POINT('Ctrl Pts',(6.94458082712411,307.223925943689,3.97163317015235));
#10974=CARTESIAN_POINT('Ctrl Pts',(5.88038492654913,307.361425943689,5.83242799455291));
#10975=CARTESIAN_POINT('Ctrl Pts',(4.02836682984766,307.498925943689,6.91182563342691));
#10976=CARTESIAN_POINT('Ctrl Pts',(2.17634873314619,307.636425943689,7.99122327230091));
#10977=CARTESIAN_POINT('Ctrl Pts',(0.0327551936971994,307.773925943689,
8.));
#10978=CARTESIAN_POINT('Ctrl Pts',(-2.11083834575178,307.911425943689,8.00877672769909));
#10979=CARTESIAN_POINT('Ctrl Pts',(-3.97163317015234,308.048925943689,6.94458082712412));
#10980=CARTESIAN_POINT('Ctrl Pts',(-5.83242799455291,308.186425943689,5.88038492654913));
#10981=CARTESIAN_POINT('Ctrl Pts',(-6.91182563342691,308.323925943689,4.02836682984766));
#10982=CARTESIAN_POINT('Ctrl Pts',(-7.99122327230091,308.461425943689,2.17634873314619));
#10983=CARTESIAN_POINT('Ctrl Pts',(-8.,308.598925943689,0.0327551936971979));
#10984=CARTESIAN_POINT('Ctrl Pts',(-8.00877672769909,308.736425943689,-2.11083834575178));
#10985=CARTESIAN_POINT('Ctrl Pts',(-6.94458082712411,308.873925943689,-3.97163317015235));
#10986=CARTESIAN_POINT('Ctrl Pts',(-5.88038492654913,309.011425943689,-5.83242799455291));
#10987=CARTESIAN_POINT('Ctrl Pts',(-4.02836682984766,309.148925943689,-6.91182563342691));
#10988=CARTESIAN_POINT('Ctrl Pts',(-2.17634873314618,309.286425943689,-7.99122327230091));
#10989=CARTESIAN_POINT('Ctrl Pts',(-0.0327551936971984,309.423925943689,
-8.));
#10990=CARTESIAN_POINT('Ctrl Pts',(2.11083834575178,309.561425943689,-8.00877672769909));
#10991=CARTESIAN_POINT('Ctrl Pts',(3.97163317015235,309.698925943689,-6.94458082712411));
#10992=CARTESIAN_POINT('Ctrl Pts',(5.83242799455291,309.836425943689,-5.88038492654913));
#10993=CARTESIAN_POINT('Ctrl Pts',(6.91182563342691,309.973925943689,-4.02836682984766));
#10994=CARTESIAN_POINT('Ctrl Pts',(7.99122327230091,310.111425943689,-2.17634873314618));
#10995=CARTESIAN_POINT('Ctrl Pts',(8.,310.248925943689,-0.0327551936971989));
#10996=CARTESIAN_POINT('Ctrl Pts',(8.00877672769909,310.386425943689,2.11083834575178));
#10997=CARTESIAN_POINT('Ctrl Pts',(6.94458082712411,310.523925943689,3.97163317015235));
#10998=CARTESIAN_POINT('Ctrl Pts',(5.88038492654913,310.661425943689,5.83242799455291));
#10999=CARTESIAN_POINT('Ctrl Pts',(4.02836682984766,310.798925943689,6.91182563342691));
#11000=CARTESIAN_POINT('Ctrl Pts',(2.17634873314619,310.936425943689,7.99122327230091));
#11001=CARTESIAN_POINT('Ctrl Pts',(0.0327551936971994,311.073925943689,
8.));
#11002=CARTESIAN_POINT('Ctrl Pts',(-2.11083834575178,311.211425943689,8.00877672769909));
#11003=CARTESIAN_POINT('Ctrl Pts',(-3.97163317015234,311.348925943689,6.94458082712412));
#11004=CARTESIAN_POINT('Ctrl Pts',(-5.83242799455291,311.486425943689,5.88038492654913));
#11005=CARTESIAN_POINT('Ctrl Pts',(-6.91182563342691,311.623925943689,4.02836682984766));
#11006=CARTESIAN_POINT('Ctrl Pts',(-7.99122327230091,311.761425943689,2.17634873314619));
#11007=CARTESIAN_POINT('Ctrl Pts',(-8.,311.898925943689,0.0327551936971979));
#11008=CARTESIAN_POINT('Ctrl Pts',(-8.00877672769909,312.036425943689,-2.11083834575178));
#11009=CARTESIAN_POINT('Ctrl Pts',(-6.94458082712411,312.173925943689,-3.97163317015235));
#11010=CARTESIAN_POINT('Ctrl Pts',(-5.88038492654913,312.311425943689,-5.83242799455291));
#11011=CARTESIAN_POINT('Ctrl Pts',(-4.02836682984766,312.448925943689,-6.91182563342691));
#11012=CARTESIAN_POINT('Ctrl Pts',(-2.17634873314618,312.586425943689,-7.99122327230091));
#11013=CARTESIAN_POINT('Ctrl Pts',(-0.0327551936971984,312.723925943689,
-8.));
#11014=CARTESIAN_POINT('Ctrl Pts',(2.11083834575178,312.861425943689,-8.00877672769909));
#11015=CARTESIAN_POINT('Ctrl Pts',(3.97163317015235,312.998925943689,-6.94458082712411));
#11016=CARTESIAN_POINT('Ctrl Pts',(5.83242799455291,313.136425943689,-5.88038492654913));
#11017=CARTESIAN_POINT('Ctrl Pts',(6.91182563342691,313.273925943689,-4.02836682984766));
#11018=CARTESIAN_POINT('Ctrl Pts',(7.99122327230091,313.411425943689,-2.17634873314618));
#11019=CARTESIAN_POINT('Ctrl Pts',(8.,313.548925943689,-0.0327551936971989));
#11020=CARTESIAN_POINT('Ctrl Pts',(8.00877672769909,313.686425943689,2.11083834575178));
#11021=CARTESIAN_POINT('Ctrl Pts',(6.94458082712411,313.823925943689,3.97163317015235));
#11022=CARTESIAN_POINT('Ctrl Pts',(5.88038492654913,313.961425943689,5.83242799455291));
#11023=CARTESIAN_POINT('Ctrl Pts',(4.02836682984766,314.098925943689,6.91182563342691));
#11024=CARTESIAN_POINT('Ctrl Pts',(2.17634873314619,314.236425943689,7.99122327230091));
#11025=CARTESIAN_POINT('Ctrl Pts',(0.0327551936971994,314.373925943689,
8.));
#11026=CARTESIAN_POINT('Ctrl Pts',(-2.11083834575178,314.511425943689,8.00877672769909));
#11027=CARTESIAN_POINT('Ctrl Pts',(-3.97163317015234,314.648925943689,6.94458082712412));
#11028=CARTESIAN_POINT('Ctrl Pts',(-5.83242799455291,314.786425943689,5.88038492654913));
#11029=CARTESIAN_POINT('Ctrl Pts',(-6.91182563342691,314.923925943689,4.02836682984766));
#11030=CARTESIAN_POINT('Ctrl Pts',(-7.99122327230091,315.061425943689,2.17634873314619));
#11031=CARTESIAN_POINT('Ctrl Pts',(-8.,315.198925943689,0.0327551936971979));
#11032=CARTESIAN_POINT('Ctrl Pts',(-8.00877672769909,315.336425943689,-2.11083834575178));
#11033=CARTESIAN_POINT('Ctrl Pts',(-6.94458082712411,315.473925943689,-3.97163317015235));
#11034=CARTESIAN_POINT('Ctrl Pts',(-5.88038492654913,315.611425943689,-5.83242799455291));
#11035=CARTESIAN_POINT('Ctrl Pts',(-4.02836682984766,315.748925943689,-6.91182563342691));
#11036=CARTESIAN_POINT('Ctrl Pts',(-2.17634873314618,315.886425943689,-7.99122327230091));
#11037=CARTESIAN_POINT('Ctrl Pts',(-0.0327551936971984,316.023925943689,
-8.));
#11038=CARTESIAN_POINT('Ctrl Pts',(2.11083834575178,316.161425943689,-8.00877672769909));
#11039=CARTESIAN_POINT('Ctrl Pts',(3.97163317015235,316.298925943689,-6.94458082712411));
#11040=CARTESIAN_POINT('Ctrl Pts',(5.83242799455291,316.436425943689,-5.88038492654913));
#11041=CARTESIAN_POINT('Ctrl Pts',(6.91182563342691,316.573925943689,-4.02836682984766));
#11042=CARTESIAN_POINT('Ctrl Pts',(7.99122327230091,316.711425943689,-2.17634873314618));
#11043=CARTESIAN_POINT('Ctrl Pts',(8.,316.848925943689,-0.0327551936971989));
#11044=CARTESIAN_POINT('Ctrl Pts',(8.00877672769909,316.986425943689,2.11083834575178));
#11045=CARTESIAN_POINT('Ctrl Pts',(6.94458082712411,317.123925943689,3.97163317015235));
#11046=CARTESIAN_POINT('Ctrl Pts',(5.88038492654913,317.261425943689,5.83242799455291));
#11047=CARTESIAN_POINT('Ctrl Pts',(4.02836682984766,317.398925943689,6.91182563342691));
#11048=CARTESIAN_POINT('Ctrl Pts',(2.17634873314619,317.536425943689,7.99122327230091));
#11049=CARTESIAN_POINT('Ctrl Pts',(0.0327551936971994,317.673925943689,
8.));
#11050=CARTESIAN_POINT('Ctrl Pts',(-2.11083834575178,317.811425943689,8.00877672769909));
#11051=CARTESIAN_POINT('Ctrl Pts',(-3.97163317015234,317.948925943689,6.94458082712412));
#11052=CARTESIAN_POINT('Ctrl Pts',(-5.83242799455291,318.086425943689,5.88038492654913));
#11053=CARTESIAN_POINT('Ctrl Pts',(-6.91182563342691,318.223925943689,4.02836682984766));
#11054=CARTESIAN_POINT('Ctrl Pts',(-7.99122327230091,318.361425943689,2.17634873314619));
#11055=CARTESIAN_POINT('Ctrl Pts',(-8.,318.498925943689,0.0327551936971979));
#11056=CARTESIAN_POINT('',(-7.50000000000002,285.,7.09974019720158E-14));
#11057=CARTESIAN_POINT('',(-4.63461213585577,285.,-6.52084682022915));
#11058=CARTESIAN_POINT('Ctrl Pts',(-7.50000000000001,285.,6.80011602582908E-14));
#11059=CARTESIAN_POINT('Ctrl Pts',(-7.50000000000002,285.,-0.640878818835817));
#11060=CARTESIAN_POINT('Ctrl Pts',(-7.42362312326954,284.999999999915,-1.27925531817836));
#11061=CARTESIAN_POINT('Ctrl Pts',(-7.13891193975039,284.999999999915,-2.46203415496977));
#11062=CARTESIAN_POINT('Ctrl Pts',(-6.94590651594617,285.,-3.00519525865999));
#11063=CARTESIAN_POINT('Ctrl Pts',(-6.26573749532748,285.,-4.43472731642613));
#11064=CARTESIAN_POINT('Ctrl Pts',(-5.73854794084772,285.,-5.12189946350785));
#11065=CARTESIAN_POINT('Ctrl Pts',(-5.09309463692861,285.,-5.88949436501166));
#11066=CARTESIAN_POINT('Ctrl Pts',(-4.87997203238035,285.,-6.11853899605642));
#11067=CARTESIAN_POINT('Ctrl Pts',(-4.70123367905775,285.,-6.34515496162355));
#11068=CARTESIAN_POINT('Ctrl Pts',(-4.66326630707557,284.999999999928,-6.39956489306395));
#11069=CARTESIAN_POINT('Ctrl Pts',(-4.63521738668531,284.999999999928,-6.45935774756588));
#11070=CARTESIAN_POINT('Ctrl Pts',(-4.6295370291925,285.,-6.47584643979257));
#11071=CARTESIAN_POINT('Ctrl Pts',(-4.6275602093536,285.,-6.49596857752024));
#11072=CARTESIAN_POINT('Ctrl Pts',(-4.62763059707101,285.,-6.50190778381856));
#11073=CARTESIAN_POINT('Ctrl Pts',(-4.62938802811186,285.,-6.51001336052072));
#11074=CARTESIAN_POINT('Ctrl Pts',(-4.63013379953918,285.,-6.51240227717505));
#11075=CARTESIAN_POINT('Ctrl Pts',(-4.63207907295903,285.,-6.51687345550803));
#11076=CARTESIAN_POINT('Ctrl Pts',(-4.63323085894002,285.,-6.51892013394952));
#11077=CARTESIAN_POINT('Ctrl Pts',(-4.63461213585325,285.,-6.52084682023095));
#11078=CARTESIAN_POINT('',(-8.,317.501074056311,-0.0327551936970314));
#11079=CARTESIAN_POINT('Ctrl Pts',(-4.63461213585577,285.,-6.52084682022915));
#11080=CARTESIAN_POINT('Ctrl Pts',(-4.31355406079092,285.025808443012,-6.7490349209516));
#11081=CARTESIAN_POINT('Ctrl Pts',(-3.97163317015249,285.051074056311,-6.94458082712403));
#11082=CARTESIAN_POINT('Ctrl Pts',(-2.11083834575195,285.188574056311,-8.00877672769905));
#11083=CARTESIAN_POINT('Ctrl Pts',(0.0327551936970309,285.326074056311,
-8.));
#11084=CARTESIAN_POINT('Ctrl Pts',(2.17634873314601,285.463574056311,-7.99122327230096));
#11085=CARTESIAN_POINT('Ctrl Pts',(4.02836682984751,285.601074056311,-6.911825633427));
#11086=CARTESIAN_POINT('Ctrl Pts',(5.88038492654901,285.738574056311,-5.83242799455303));
#11087=CARTESIAN_POINT('Ctrl Pts',(6.94458082712403,285.876074056311,-3.9716331701525));
#11088=CARTESIAN_POINT('Ctrl Pts',(8.00877672769905,286.013574056311,-2.11083834575195));
#11089=CARTESIAN_POINT('Ctrl Pts',(8.,286.151074056311,0.0327551936970304));
#11090=CARTESIAN_POINT('Ctrl Pts',(7.99122327230096,286.288574056311,2.17634873314601));
#11091=CARTESIAN_POINT('Ctrl Pts',(6.911825633427,286.426074056311,4.02836682984751));
#11092=CARTESIAN_POINT('Ctrl Pts',(5.83242799455304,286.563574056311,5.880384926549));
#11093=CARTESIAN_POINT('Ctrl Pts',(3.9716331701525,286.701074056311,6.94458082712403));
#11094=CARTESIAN_POINT('Ctrl Pts',(2.11083834575196,286.838574056311,8.00877672769905));
#11095=CARTESIAN_POINT('Ctrl Pts',(-0.0327551936970299,286.976074056311,
8.));
#11096=CARTESIAN_POINT('Ctrl Pts',(-2.17634873314601,287.113574056311,7.99122327230096));
#11097=CARTESIAN_POINT('Ctrl Pts',(-4.02836682984751,287.251074056311,6.911825633427));
#11098=CARTESIAN_POINT('Ctrl Pts',(-5.88038492654901,287.388574056311,5.83242799455303));
#11099=CARTESIAN_POINT('Ctrl Pts',(-6.94458082712403,287.526074056311,3.9716331701525));
#11100=CARTESIAN_POINT('Ctrl Pts',(-8.00877672769905,287.663574056311,2.11083834575196));
#11101=CARTESIAN_POINT('Ctrl Pts',(-8.,287.801074056311,-0.0327551936970314));
#11102=CARTESIAN_POINT('Ctrl Pts',(-7.99122327230096,287.938574056311,-2.17634873314601));
#11103=CARTESIAN_POINT('Ctrl Pts',(-6.911825633427,288.076074056311,-4.02836682984751));
#11104=CARTESIAN_POINT('Ctrl Pts',(-5.83242799455303,288.213574056311,-5.88038492654901));
#11105=CARTESIAN_POINT('Ctrl Pts',(-3.97163317015249,288.351074056311,-6.94458082712403));
#11106=CARTESIAN_POINT('Ctrl Pts',(-2.11083834575195,288.488574056311,-8.00877672769905));
#11107=CARTESIAN_POINT('Ctrl Pts',(0.0327551936970309,288.626074056311,
-8.));
#11108=CARTESIAN_POINT('Ctrl Pts',(2.17634873314601,288.763574056311,-7.99122327230096));
#11109=CARTESIAN_POINT('Ctrl Pts',(4.02836682984751,288.901074056311,-6.911825633427));
#11110=CARTESIAN_POINT('Ctrl Pts',(5.88038492654901,289.038574056311,-5.83242799455303));
#11111=CARTESIAN_POINT('Ctrl Pts',(6.94458082712403,289.176074056311,-3.9716331701525));
#11112=CARTESIAN_POINT('Ctrl Pts',(8.00877672769905,289.313574056311,-2.11083834575195));
#11113=CARTESIAN_POINT('Ctrl Pts',(8.,289.451074056311,0.0327551936970304));
#11114=CARTESIAN_POINT('Ctrl Pts',(7.99122327230096,289.588574056311,2.17634873314601));
#11115=CARTESIAN_POINT('Ctrl Pts',(6.911825633427,289.726074056311,4.02836682984751));
#11116=CARTESIAN_POINT('Ctrl Pts',(5.83242799455304,289.863574056311,5.880384926549));
#11117=CARTESIAN_POINT('Ctrl Pts',(3.9716331701525,290.001074056311,6.94458082712403));
#11118=CARTESIAN_POINT('Ctrl Pts',(2.11083834575196,290.138574056311,8.00877672769905));
#11119=CARTESIAN_POINT('Ctrl Pts',(-0.0327551936970299,290.276074056311,
8.));
#11120=CARTESIAN_POINT('Ctrl Pts',(-2.17634873314601,290.413574056311,7.99122327230096));
#11121=CARTESIAN_POINT('Ctrl Pts',(-4.02836682984751,290.551074056311,6.911825633427));
#11122=CARTESIAN_POINT('Ctrl Pts',(-5.88038492654901,290.688574056311,5.83242799455303));
#11123=CARTESIAN_POINT('Ctrl Pts',(-6.94458082712403,290.826074056311,3.9716331701525));
#11124=CARTESIAN_POINT('Ctrl Pts',(-8.00877672769905,290.963574056311,2.11083834575196));
#11125=CARTESIAN_POINT('Ctrl Pts',(-8.,291.101074056311,-0.0327551936970314));
#11126=CARTESIAN_POINT('Ctrl Pts',(-7.99122327230096,291.238574056311,-2.17634873314601));
#11127=CARTESIAN_POINT('Ctrl Pts',(-6.911825633427,291.376074056311,-4.02836682984751));
#11128=CARTESIAN_POINT('Ctrl Pts',(-5.83242799455303,291.513574056311,-5.88038492654901));
#11129=CARTESIAN_POINT('Ctrl Pts',(-3.97163317015249,291.651074056311,-6.94458082712403));
#11130=CARTESIAN_POINT('Ctrl Pts',(-2.11083834575195,291.788574056311,-8.00877672769905));
#11131=CARTESIAN_POINT('Ctrl Pts',(0.0327551936970309,291.926074056311,
-8.));
#11132=CARTESIAN_POINT('Ctrl Pts',(2.17634873314601,292.063574056311,-7.99122327230096));
#11133=CARTESIAN_POINT('Ctrl Pts',(4.02836682984751,292.201074056311,-6.911825633427));
#11134=CARTESIAN_POINT('Ctrl Pts',(5.88038492654901,292.338574056311,-5.83242799455303));
#11135=CARTESIAN_POINT('Ctrl Pts',(6.94458082712403,292.476074056311,-3.9716331701525));
#11136=CARTESIAN_POINT('Ctrl Pts',(8.00877672769905,292.613574056311,-2.11083834575195));
#11137=CARTESIAN_POINT('Ctrl Pts',(8.,292.751074056311,0.0327551936970304));
#11138=CARTESIAN_POINT('Ctrl Pts',(7.99122327230096,292.888574056311,2.17634873314601));
#11139=CARTESIAN_POINT('Ctrl Pts',(6.911825633427,293.026074056311,4.02836682984751));
#11140=CARTESIAN_POINT('Ctrl Pts',(5.83242799455304,293.163574056311,5.880384926549));
#11141=CARTESIAN_POINT('Ctrl Pts',(3.9716331701525,293.301074056311,6.94458082712403));
#11142=CARTESIAN_POINT('Ctrl Pts',(2.11083834575196,293.438574056311,8.00877672769905));
#11143=CARTESIAN_POINT('Ctrl Pts',(-0.0327551936970299,293.576074056311,
8.));
#11144=CARTESIAN_POINT('Ctrl Pts',(-2.17634873314601,293.713574056311,7.99122327230096));
#11145=CARTESIAN_POINT('Ctrl Pts',(-4.02836682984751,293.851074056311,6.911825633427));
#11146=CARTESIAN_POINT('Ctrl Pts',(-5.88038492654901,293.988574056311,5.83242799455303));
#11147=CARTESIAN_POINT('Ctrl Pts',(-6.94458082712403,294.126074056311,3.9716331701525));
#11148=CARTESIAN_POINT('Ctrl Pts',(-8.00877672769905,294.263574056311,2.11083834575196));
#11149=CARTESIAN_POINT('Ctrl Pts',(-8.,294.401074056311,-0.0327551936970314));
#11150=CARTESIAN_POINT('Ctrl Pts',(-7.99122327230096,294.538574056311,-2.17634873314601));
#11151=CARTESIAN_POINT('Ctrl Pts',(-6.911825633427,294.676074056311,-4.02836682984751));
#11152=CARTESIAN_POINT('Ctrl Pts',(-5.83242799455303,294.813574056311,-5.88038492654901));
#11153=CARTESIAN_POINT('Ctrl Pts',(-3.97163317015249,294.951074056311,-6.94458082712403));
#11154=CARTESIAN_POINT('Ctrl Pts',(-2.11083834575195,295.088574056311,-8.00877672769905));
#11155=CARTESIAN_POINT('Ctrl Pts',(0.0327551936970309,295.226074056311,
-8.));
#11156=CARTESIAN_POINT('Ctrl Pts',(2.17634873314601,295.363574056311,-7.99122327230096));
#11157=CARTESIAN_POINT('Ctrl Pts',(4.02836682984751,295.501074056311,-6.911825633427));
#11158=CARTESIAN_POINT('Ctrl Pts',(5.88038492654901,295.638574056311,-5.83242799455303));
#11159=CARTESIAN_POINT('Ctrl Pts',(6.94458082712403,295.776074056311,-3.9716331701525));
#11160=CARTESIAN_POINT('Ctrl Pts',(8.00877672769905,295.913574056311,-2.11083834575195));
#11161=CARTESIAN_POINT('Ctrl Pts',(8.,296.051074056311,0.0327551936970304));
#11162=CARTESIAN_POINT('Ctrl Pts',(7.99122327230096,296.188574056311,2.17634873314601));
#11163=CARTESIAN_POINT('Ctrl Pts',(6.911825633427,296.326074056311,4.02836682984751));
#11164=CARTESIAN_POINT('Ctrl Pts',(5.83242799455304,296.463574056311,5.880384926549));
#11165=CARTESIAN_POINT('Ctrl Pts',(3.9716331701525,296.601074056311,6.94458082712403));
#11166=CARTESIAN_POINT('Ctrl Pts',(2.11083834575196,296.738574056311,8.00877672769905));
#11167=CARTESIAN_POINT('Ctrl Pts',(-0.0327551936970299,296.876074056311,
8.));
#11168=CARTESIAN_POINT('Ctrl Pts',(-2.17634873314601,297.013574056311,7.99122327230096));
#11169=CARTESIAN_POINT('Ctrl Pts',(-4.02836682984751,297.151074056311,6.911825633427));
#11170=CARTESIAN_POINT('Ctrl Pts',(-5.88038492654901,297.288574056311,5.83242799455303));
#11171=CARTESIAN_POINT('Ctrl Pts',(-6.94458082712403,297.426074056311,3.9716331701525));
#11172=CARTESIAN_POINT('Ctrl Pts',(-8.00877672769905,297.563574056311,2.11083834575196));
#11173=CARTESIAN_POINT('Ctrl Pts',(-8.,297.701074056311,-0.0327551936970314));
#11174=CARTESIAN_POINT('Ctrl Pts',(-7.99122327230096,297.838574056311,-2.17634873314601));
#11175=CARTESIAN_POINT('Ctrl Pts',(-6.911825633427,297.976074056311,-4.02836682984751));
#11176=CARTESIAN_POINT('Ctrl Pts',(-5.83242799455303,298.113574056311,-5.88038492654901));
#11177=CARTESIAN_POINT('Ctrl Pts',(-3.97163317015249,298.251074056311,-6.94458082712403));
#11178=CARTESIAN_POINT('Ctrl Pts',(-2.11083834575195,298.388574056311,-8.00877672769905));
#11179=CARTESIAN_POINT('Ctrl Pts',(0.0327551936970309,298.526074056311,
-8.));
#11180=CARTESIAN_POINT('Ctrl Pts',(2.17634873314601,298.663574056311,-7.99122327230096));
#11181=CARTESIAN_POINT('Ctrl Pts',(4.02836682984751,298.801074056311,-6.911825633427));
#11182=CARTESIAN_POINT('Ctrl Pts',(5.88038492654901,298.938574056311,-5.83242799455303));
#11183=CARTESIAN_POINT('Ctrl Pts',(6.94458082712403,299.076074056311,-3.9716331701525));
#11184=CARTESIAN_POINT('Ctrl Pts',(8.00877672769905,299.213574056311,-2.11083834575195));
#11185=CARTESIAN_POINT('Ctrl Pts',(8.,299.351074056311,0.0327551936970304));
#11186=CARTESIAN_POINT('Ctrl Pts',(7.99122327230096,299.488574056311,2.17634873314601));
#11187=CARTESIAN_POINT('Ctrl Pts',(6.911825633427,299.626074056311,4.02836682984751));
#11188=CARTESIAN_POINT('Ctrl Pts',(5.83242799455304,299.763574056311,5.880384926549));
#11189=CARTESIAN_POINT('Ctrl Pts',(3.9716331701525,299.901074056311,6.94458082712403));
#11190=CARTESIAN_POINT('Ctrl Pts',(2.11083834575196,300.038574056311,8.00877672769905));
#11191=CARTESIAN_POINT('Ctrl Pts',(-0.0327551936970299,300.176074056311,
8.));
#11192=CARTESIAN_POINT('Ctrl Pts',(-2.17634873314601,300.313574056311,7.99122327230096));
#11193=CARTESIAN_POINT('Ctrl Pts',(-4.02836682984751,300.451074056311,6.911825633427));
#11194=CARTESIAN_POINT('Ctrl Pts',(-5.88038492654901,300.588574056311,5.83242799455303));
#11195=CARTESIAN_POINT('Ctrl Pts',(-6.94458082712403,300.726074056311,3.9716331701525));
#11196=CARTESIAN_POINT('Ctrl Pts',(-8.00877672769905,300.863574056311,2.11083834575196));
#11197=CARTESIAN_POINT('Ctrl Pts',(-8.,301.001074056311,-0.0327551936970314));
#11198=CARTESIAN_POINT('Ctrl Pts',(-7.99122327230096,301.138574056311,-2.17634873314601));
#11199=CARTESIAN_POINT('Ctrl Pts',(-6.911825633427,301.276074056311,-4.02836682984751));
#11200=CARTESIAN_POINT('Ctrl Pts',(-5.83242799455303,301.413574056311,-5.88038492654901));
#11201=CARTESIAN_POINT('Ctrl Pts',(-3.97163317015249,301.551074056311,-6.94458082712403));
#11202=CARTESIAN_POINT('Ctrl Pts',(-2.11083834575195,301.688574056311,-8.00877672769905));
#11203=CARTESIAN_POINT('Ctrl Pts',(0.0327551936970309,301.826074056311,
-8.));
#11204=CARTESIAN_POINT('Ctrl Pts',(2.17634873314601,301.963574056311,-7.99122327230096));
#11205=CARTESIAN_POINT('Ctrl Pts',(4.02836682984751,302.101074056311,-6.911825633427));
#11206=CARTESIAN_POINT('Ctrl Pts',(5.88038492654901,302.238574056311,-5.83242799455303));
#11207=CARTESIAN_POINT('Ctrl Pts',(6.94458082712403,302.376074056311,-3.9716331701525));
#11208=CARTESIAN_POINT('Ctrl Pts',(8.00877672769905,302.513574056311,-2.11083834575195));
#11209=CARTESIAN_POINT('Ctrl Pts',(8.,302.651074056311,0.0327551936970304));
#11210=CARTESIAN_POINT('Ctrl Pts',(7.99122327230096,302.788574056311,2.17634873314601));
#11211=CARTESIAN_POINT('Ctrl Pts',(6.911825633427,302.926074056311,4.02836682984751));
#11212=CARTESIAN_POINT('Ctrl Pts',(5.83242799455304,303.063574056311,5.880384926549));
#11213=CARTESIAN_POINT('Ctrl Pts',(3.9716331701525,303.201074056311,6.94458082712403));
#11214=CARTESIAN_POINT('Ctrl Pts',(2.11083834575196,303.338574056311,8.00877672769905));
#11215=CARTESIAN_POINT('Ctrl Pts',(-0.0327551936970299,303.476074056311,
8.));
#11216=CARTESIAN_POINT('Ctrl Pts',(-2.17634873314601,303.613574056311,7.99122327230096));
#11217=CARTESIAN_POINT('Ctrl Pts',(-4.02836682984751,303.751074056311,6.911825633427));
#11218=CARTESIAN_POINT('Ctrl Pts',(-5.88038492654901,303.888574056311,5.83242799455303));
#11219=CARTESIAN_POINT('Ctrl Pts',(-6.94458082712403,304.026074056311,3.9716331701525));
#11220=CARTESIAN_POINT('Ctrl Pts',(-8.00877672769905,304.163574056311,2.11083834575196));
#11221=CARTESIAN_POINT('Ctrl Pts',(-8.,304.301074056311,-0.0327551936970314));
#11222=CARTESIAN_POINT('Ctrl Pts',(-7.99122327230096,304.438574056311,-2.17634873314601));
#11223=CARTESIAN_POINT('Ctrl Pts',(-6.911825633427,304.576074056311,-4.02836682984751));
#11224=CARTESIAN_POINT('Ctrl Pts',(-5.83242799455303,304.713574056311,-5.88038492654901));
#11225=CARTESIAN_POINT('Ctrl Pts',(-3.97163317015249,304.851074056311,-6.94458082712403));
#11226=CARTESIAN_POINT('Ctrl Pts',(-2.11083834575195,304.988574056311,-8.00877672769905));
#11227=CARTESIAN_POINT('Ctrl Pts',(0.0327551936970309,305.126074056311,
-8.));
#11228=CARTESIAN_POINT('Ctrl Pts',(2.17634873314601,305.263574056311,-7.99122327230096));
#11229=CARTESIAN_POINT('Ctrl Pts',(4.02836682984751,305.401074056311,-6.911825633427));
#11230=CARTESIAN_POINT('Ctrl Pts',(5.88038492654901,305.538574056311,-5.83242799455303));
#11231=CARTESIAN_POINT('Ctrl Pts',(6.94458082712403,305.676074056311,-3.9716331701525));
#11232=CARTESIAN_POINT('Ctrl Pts',(8.00877672769905,305.813574056311,-2.11083834575195));
#11233=CARTESIAN_POINT('Ctrl Pts',(8.,305.951074056311,0.0327551936970304));
#11234=CARTESIAN_POINT('Ctrl Pts',(7.99122327230096,306.088574056311,2.17634873314601));
#11235=CARTESIAN_POINT('Ctrl Pts',(6.911825633427,306.226074056311,4.02836682984751));
#11236=CARTESIAN_POINT('Ctrl Pts',(5.83242799455304,306.363574056311,5.880384926549));
#11237=CARTESIAN_POINT('Ctrl Pts',(3.9716331701525,306.501074056311,6.94458082712403));
#11238=CARTESIAN_POINT('Ctrl Pts',(2.11083834575196,306.638574056311,8.00877672769905));
#11239=CARTESIAN_POINT('Ctrl Pts',(-0.0327551936970299,306.776074056311,
8.));
#11240=CARTESIAN_POINT('Ctrl Pts',(-2.17634873314601,306.913574056311,7.99122327230096));
#11241=CARTESIAN_POINT('Ctrl Pts',(-4.02836682984751,307.051074056311,6.911825633427));
#11242=CARTESIAN_POINT('Ctrl Pts',(-5.88038492654901,307.188574056311,5.83242799455303));
#11243=CARTESIAN_POINT('Ctrl Pts',(-6.94458082712403,307.326074056311,3.9716331701525));
#11244=CARTESIAN_POINT('Ctrl Pts',(-8.00877672769905,307.463574056311,2.11083834575196));
#11245=CARTESIAN_POINT('Ctrl Pts',(-8.,307.601074056311,-0.0327551936970314));
#11246=CARTESIAN_POINT('Ctrl Pts',(-7.99122327230096,307.738574056311,-2.17634873314601));
#11247=CARTESIAN_POINT('Ctrl Pts',(-6.911825633427,307.876074056311,-4.02836682984751));
#11248=CARTESIAN_POINT('Ctrl Pts',(-5.83242799455303,308.013574056311,-5.88038492654901));
#11249=CARTESIAN_POINT('Ctrl Pts',(-3.97163317015249,308.151074056311,-6.94458082712403));
#11250=CARTESIAN_POINT('Ctrl Pts',(-2.11083834575195,308.288574056311,-8.00877672769905));
#11251=CARTESIAN_POINT('Ctrl Pts',(0.0327551936970309,308.426074056311,
-8.));
#11252=CARTESIAN_POINT('Ctrl Pts',(2.17634873314601,308.563574056311,-7.99122327230096));
#11253=CARTESIAN_POINT('Ctrl Pts',(4.02836682984751,308.701074056311,-6.911825633427));
#11254=CARTESIAN_POINT('Ctrl Pts',(5.88038492654901,308.838574056311,-5.83242799455303));
#11255=CARTESIAN_POINT('Ctrl Pts',(6.94458082712403,308.976074056311,-3.9716331701525));
#11256=CARTESIAN_POINT('Ctrl Pts',(8.00877672769905,309.113574056311,-2.11083834575195));
#11257=CARTESIAN_POINT('Ctrl Pts',(8.,309.251074056311,0.0327551936970304));
#11258=CARTESIAN_POINT('Ctrl Pts',(7.99122327230096,309.388574056311,2.17634873314601));
#11259=CARTESIAN_POINT('Ctrl Pts',(6.911825633427,309.526074056311,4.02836682984751));
#11260=CARTESIAN_POINT('Ctrl Pts',(5.83242799455304,309.663574056311,5.880384926549));
#11261=CARTESIAN_POINT('Ctrl Pts',(3.9716331701525,309.801074056311,6.94458082712403));
#11262=CARTESIAN_POINT('Ctrl Pts',(2.11083834575196,309.938574056311,8.00877672769905));
#11263=CARTESIAN_POINT('Ctrl Pts',(-0.0327551936970299,310.076074056311,
8.));
#11264=CARTESIAN_POINT('Ctrl Pts',(-2.17634873314601,310.213574056311,7.99122327230096));
#11265=CARTESIAN_POINT('Ctrl Pts',(-4.02836682984751,310.351074056311,6.911825633427));
#11266=CARTESIAN_POINT('Ctrl Pts',(-5.88038492654901,310.488574056311,5.83242799455303));
#11267=CARTESIAN_POINT('Ctrl Pts',(-6.94458082712403,310.626074056311,3.9716331701525));
#11268=CARTESIAN_POINT('Ctrl Pts',(-8.00877672769905,310.763574056311,2.11083834575196));
#11269=CARTESIAN_POINT('Ctrl Pts',(-8.,310.901074056311,-0.0327551936970314));
#11270=CARTESIAN_POINT('Ctrl Pts',(-7.99122327230096,311.038574056311,-2.17634873314601));
#11271=CARTESIAN_POINT('Ctrl Pts',(-6.911825633427,311.176074056311,-4.02836682984751));
#11272=CARTESIAN_POINT('Ctrl Pts',(-5.83242799455303,311.313574056311,-5.88038492654901));
#11273=CARTESIAN_POINT('Ctrl Pts',(-3.97163317015249,311.451074056311,-6.94458082712403));
#11274=CARTESIAN_POINT('Ctrl Pts',(-2.11083834575195,311.588574056311,-8.00877672769905));
#11275=CARTESIAN_POINT('Ctrl Pts',(0.0327551936970309,311.726074056311,
-8.));
#11276=CARTESIAN_POINT('Ctrl Pts',(2.17634873314601,311.863574056311,-7.99122327230096));
#11277=CARTESIAN_POINT('Ctrl Pts',(4.02836682984751,312.001074056311,-6.911825633427));
#11278=CARTESIAN_POINT('Ctrl Pts',(5.88038492654901,312.138574056311,-5.83242799455303));
#11279=CARTESIAN_POINT('Ctrl Pts',(6.94458082712403,312.276074056311,-3.9716331701525));
#11280=CARTESIAN_POINT('Ctrl Pts',(8.00877672769905,312.413574056311,-2.11083834575195));
#11281=CARTESIAN_POINT('Ctrl Pts',(8.,312.551074056311,0.0327551936970304));
#11282=CARTESIAN_POINT('Ctrl Pts',(7.99122327230096,312.688574056311,2.17634873314601));
#11283=CARTESIAN_POINT('Ctrl Pts',(6.911825633427,312.826074056311,4.02836682984751));
#11284=CARTESIAN_POINT('Ctrl Pts',(5.83242799455304,312.963574056311,5.880384926549));
#11285=CARTESIAN_POINT('Ctrl Pts',(3.9716331701525,313.101074056311,6.94458082712403));
#11286=CARTESIAN_POINT('Ctrl Pts',(2.11083834575196,313.238574056311,8.00877672769905));
#11287=CARTESIAN_POINT('Ctrl Pts',(-0.0327551936970299,313.376074056311,
8.));
#11288=CARTESIAN_POINT('Ctrl Pts',(-2.17634873314601,313.513574056311,7.99122327230096));
#11289=CARTESIAN_POINT('Ctrl Pts',(-4.02836682984751,313.651074056311,6.911825633427));
#11290=CARTESIAN_POINT('Ctrl Pts',(-5.88038492654901,313.788574056311,5.83242799455303));
#11291=CARTESIAN_POINT('Ctrl Pts',(-6.94458082712403,313.926074056311,3.9716331701525));
#11292=CARTESIAN_POINT('Ctrl Pts',(-8.00877672769905,314.063574056311,2.11083834575196));
#11293=CARTESIAN_POINT('Ctrl Pts',(-8.,314.201074056311,-0.0327551936970314));
#11294=CARTESIAN_POINT('Ctrl Pts',(-7.99122327230096,314.338574056311,-2.17634873314601));
#11295=CARTESIAN_POINT('Ctrl Pts',(-6.911825633427,314.476074056311,-4.02836682984751));
#11296=CARTESIAN_POINT('Ctrl Pts',(-5.83242799455303,314.613574056311,-5.88038492654901));
#11297=CARTESIAN_POINT('Ctrl Pts',(-3.97163317015249,314.751074056311,-6.94458082712403));
#11298=CARTESIAN_POINT('Ctrl Pts',(-2.11083834575195,314.888574056311,-8.00877672769905));
#11299=CARTESIAN_POINT('Ctrl Pts',(0.0327551936970309,315.026074056311,
-8.));
#11300=CARTESIAN_POINT('Ctrl Pts',(2.17634873314601,315.163574056311,-7.99122327230096));
#11301=CARTESIAN_POINT('Ctrl Pts',(4.02836682984751,315.301074056311,-6.911825633427));
#11302=CARTESIAN_POINT('Ctrl Pts',(5.88038492654901,315.438574056311,-5.83242799455303));
#11303=CARTESIAN_POINT('Ctrl Pts',(6.94458082712403,315.576074056311,-3.9716331701525));
#11304=CARTESIAN_POINT('Ctrl Pts',(8.00877672769905,315.713574056311,-2.11083834575195));
#11305=CARTESIAN_POINT('Ctrl Pts',(8.,315.851074056311,0.0327551936970304));
#11306=CARTESIAN_POINT('Ctrl Pts',(7.99122327230096,315.988574056311,2.17634873314601));
#11307=CARTESIAN_POINT('Ctrl Pts',(6.911825633427,316.126074056311,4.02836682984751));
#11308=CARTESIAN_POINT('Ctrl Pts',(5.83242799455304,316.263574056311,5.880384926549));
#11309=CARTESIAN_POINT('Ctrl Pts',(3.9716331701525,316.401074056311,6.94458082712403));
#11310=CARTESIAN_POINT('Ctrl Pts',(2.11083834575196,316.538574056311,8.00877672769905));
#11311=CARTESIAN_POINT('Ctrl Pts',(-0.0327551936970299,316.676074056311,
8.));
#11312=CARTESIAN_POINT('Ctrl Pts',(-2.17634873314601,316.813574056311,7.99122327230096));
#11313=CARTESIAN_POINT('Ctrl Pts',(-4.02836682984751,316.951074056311,6.911825633427));
#11314=CARTESIAN_POINT('Ctrl Pts',(-5.88038492654901,317.088574056311,5.83242799455303));
#11315=CARTESIAN_POINT('Ctrl Pts',(-6.94458082712403,317.226074056311,3.9716331701525));
#11316=CARTESIAN_POINT('Ctrl Pts',(-8.00877672769905,317.363574056311,2.11083834575196));
#11317=CARTESIAN_POINT('Ctrl Pts',(-8.,317.501074056311,-0.0327551936970314));
#11318=CARTESIAN_POINT('',(-8.,318.498925943689,0.0327551936971979));
#11319=CARTESIAN_POINT('Origin',(-8.,318.,8.32667268468867E-14));
#11320=CARTESIAN_POINT('',(-8.,285.498925943689,0.0327551936971979));
#11321=CARTESIAN_POINT('Ctrl Pts',(-8.,285.498925943689,0.0327551936971979));
#11322=CARTESIAN_POINT('Ctrl Pts',(-8.00877672769909,285.636425943689,-2.11083834575179));
#11323=CARTESIAN_POINT('Ctrl Pts',(-6.94458082712411,285.773925943689,-3.97163317015235));
#11324=CARTESIAN_POINT('Ctrl Pts',(-5.88038492654913,285.911425943689,-5.83242799455291));
#11325=CARTESIAN_POINT('Ctrl Pts',(-4.02836682984766,286.048925943689,-6.91182563342691));
#11326=CARTESIAN_POINT('Ctrl Pts',(-2.17634873314618,286.186425943689,-7.99122327230091));
#11327=CARTESIAN_POINT('Ctrl Pts',(-0.0327551936971984,286.323925943689,
-8.));
#11328=CARTESIAN_POINT('Ctrl Pts',(2.11083834575178,286.461425943689,-8.00877672769909));
#11329=CARTESIAN_POINT('Ctrl Pts',(3.97163317015235,286.598925943689,-6.94458082712411));
#11330=CARTESIAN_POINT('Ctrl Pts',(5.83242799455291,286.736425943689,-5.88038492654913));
#11331=CARTESIAN_POINT('Ctrl Pts',(6.91182563342691,286.873925943689,-4.02836682984766));
#11332=CARTESIAN_POINT('Ctrl Pts',(7.99122327230091,287.011425943689,-2.17634873314618));
#11333=CARTESIAN_POINT('Ctrl Pts',(8.,287.148925943689,-0.0327551936971989));
#11334=CARTESIAN_POINT('Ctrl Pts',(8.00877672769909,287.286425943689,2.11083834575178));
#11335=CARTESIAN_POINT('Ctrl Pts',(6.94458082712411,287.423925943689,3.97163317015235));
#11336=CARTESIAN_POINT('Ctrl Pts',(5.88038492654913,287.561425943689,5.83242799455291));
#11337=CARTESIAN_POINT('Ctrl Pts',(4.02836682984766,287.698925943689,6.91182563342691));
#11338=CARTESIAN_POINT('Ctrl Pts',(2.17634873314619,287.836425943689,7.99122327230091));
#11339=CARTESIAN_POINT('Ctrl Pts',(0.0327551936971994,287.973925943689,
8.));
#11340=CARTESIAN_POINT('Ctrl Pts',(-2.11083834575178,288.111425943689,8.00877672769909));
#11341=CARTESIAN_POINT('Ctrl Pts',(-3.97163317015234,288.248925943689,6.94458082712412));
#11342=CARTESIAN_POINT('Ctrl Pts',(-5.83242799455291,288.386425943689,5.88038492654913));
#11343=CARTESIAN_POINT('Ctrl Pts',(-6.91182563342691,288.523925943689,4.02836682984766));
#11344=CARTESIAN_POINT('Ctrl Pts',(-7.99122327230091,288.661425943689,2.17634873314619));
#11345=CARTESIAN_POINT('Ctrl Pts',(-8.,288.798925943689,0.0327551936971979));
#11346=CARTESIAN_POINT('Ctrl Pts',(-8.00877672769909,288.936425943689,-2.11083834575178));
#11347=CARTESIAN_POINT('Ctrl Pts',(-6.94458082712411,289.073925943689,-3.97163317015235));
#11348=CARTESIAN_POINT('Ctrl Pts',(-5.88038492654913,289.211425943689,-5.83242799455291));
#11349=CARTESIAN_POINT('Ctrl Pts',(-4.02836682984766,289.348925943689,-6.91182563342691));
#11350=CARTESIAN_POINT('Ctrl Pts',(-2.17634873314618,289.486425943689,-7.99122327230091));
#11351=CARTESIAN_POINT('Ctrl Pts',(-0.0327551936971984,289.623925943689,
-8.));
#11352=CARTESIAN_POINT('Ctrl Pts',(2.11083834575178,289.761425943689,-8.00877672769909));
#11353=CARTESIAN_POINT('Ctrl Pts',(3.97163317015235,289.898925943689,-6.94458082712411));
#11354=CARTESIAN_POINT('Ctrl Pts',(5.83242799455291,290.036425943689,-5.88038492654913));
#11355=CARTESIAN_POINT('Ctrl Pts',(6.91182563342691,290.173925943689,-4.02836682984766));
#11356=CARTESIAN_POINT('Ctrl Pts',(7.99122327230091,290.311425943689,-2.17634873314618));
#11357=CARTESIAN_POINT('Ctrl Pts',(8.,290.448925943689,-0.0327551936971989));
#11358=CARTESIAN_POINT('Ctrl Pts',(8.00877672769909,290.586425943689,2.11083834575178));
#11359=CARTESIAN_POINT('Ctrl Pts',(6.94458082712411,290.723925943689,3.97163317015235));
#11360=CARTESIAN_POINT('Ctrl Pts',(5.88038492654913,290.861425943689,5.83242799455291));
#11361=CARTESIAN_POINT('Ctrl Pts',(4.02836682984766,290.998925943689,6.91182563342691));
#11362=CARTESIAN_POINT('Ctrl Pts',(2.17634873314619,291.136425943689,7.99122327230091));
#11363=CARTESIAN_POINT('Ctrl Pts',(0.0327551936971994,291.273925943689,
8.));
#11364=CARTESIAN_POINT('Ctrl Pts',(-2.11083834575178,291.411425943689,8.00877672769909));
#11365=CARTESIAN_POINT('Ctrl Pts',(-3.97163317015234,291.548925943689,6.94458082712412));
#11366=CARTESIAN_POINT('Ctrl Pts',(-5.83242799455291,291.686425943689,5.88038492654913));
#11367=CARTESIAN_POINT('Ctrl Pts',(-6.91182563342691,291.823925943689,4.02836682984766));
#11368=CARTESIAN_POINT('Ctrl Pts',(-7.99122327230091,291.961425943689,2.17634873314619));
#11369=CARTESIAN_POINT('Ctrl Pts',(-8.,292.098925943689,0.0327551936971979));
#11370=CARTESIAN_POINT('Ctrl Pts',(-8.00877672769909,292.236425943689,-2.11083834575178));
#11371=CARTESIAN_POINT('Ctrl Pts',(-6.94458082712411,292.373925943689,-3.97163317015235));
#11372=CARTESIAN_POINT('Ctrl Pts',(-5.88038492654913,292.511425943689,-5.83242799455291));
#11373=CARTESIAN_POINT('Ctrl Pts',(-4.02836682984766,292.648925943689,-6.91182563342691));
#11374=CARTESIAN_POINT('Ctrl Pts',(-2.17634873314618,292.786425943689,-7.99122327230091));
#11375=CARTESIAN_POINT('Ctrl Pts',(-0.0327551936971984,292.923925943689,
-8.));
#11376=CARTESIAN_POINT('Ctrl Pts',(2.11083834575178,293.061425943689,-8.00877672769909));
#11377=CARTESIAN_POINT('Ctrl Pts',(3.97163317015235,293.198925943689,-6.94458082712411));
#11378=CARTESIAN_POINT('Ctrl Pts',(5.83242799455291,293.336425943689,-5.88038492654913));
#11379=CARTESIAN_POINT('Ctrl Pts',(6.91182563342691,293.473925943689,-4.02836682984766));
#11380=CARTESIAN_POINT('Ctrl Pts',(7.99122327230091,293.611425943689,-2.17634873314618));
#11381=CARTESIAN_POINT('Ctrl Pts',(8.,293.748925943689,-0.0327551936971989));
#11382=CARTESIAN_POINT('Ctrl Pts',(8.00877672769909,293.886425943689,2.11083834575178));
#11383=CARTESIAN_POINT('Ctrl Pts',(6.94458082712411,294.023925943689,3.97163317015235));
#11384=CARTESIAN_POINT('Ctrl Pts',(5.88038492654913,294.161425943689,5.83242799455291));
#11385=CARTESIAN_POINT('Ctrl Pts',(4.02836682984766,294.298925943689,6.91182563342691));
#11386=CARTESIAN_POINT('Ctrl Pts',(2.17634873314619,294.436425943689,7.99122327230091));
#11387=CARTESIAN_POINT('Ctrl Pts',(0.0327551936971994,294.573925943689,
8.));
#11388=CARTESIAN_POINT('Ctrl Pts',(-2.11083834575178,294.711425943689,8.00877672769909));
#11389=CARTESIAN_POINT('Ctrl Pts',(-3.97163317015234,294.848925943689,6.94458082712412));
#11390=CARTESIAN_POINT('Ctrl Pts',(-5.83242799455291,294.986425943689,5.88038492654913));
#11391=CARTESIAN_POINT('Ctrl Pts',(-6.91182563342691,295.123925943689,4.02836682984766));
#11392=CARTESIAN_POINT('Ctrl Pts',(-7.99122327230091,295.261425943689,2.17634873314619));
#11393=CARTESIAN_POINT('Ctrl Pts',(-8.,295.398925943689,0.0327551936971979));
#11394=CARTESIAN_POINT('Ctrl Pts',(-8.00877672769909,295.536425943689,-2.11083834575178));
#11395=CARTESIAN_POINT('Ctrl Pts',(-6.94458082712411,295.673925943689,-3.97163317015235));
#11396=CARTESIAN_POINT('Ctrl Pts',(-5.88038492654913,295.811425943689,-5.83242799455291));
#11397=CARTESIAN_POINT('Ctrl Pts',(-4.02836682984766,295.948925943689,-6.91182563342691));
#11398=CARTESIAN_POINT('Ctrl Pts',(-2.17634873314618,296.086425943689,-7.99122327230091));
#11399=CARTESIAN_POINT('Ctrl Pts',(-0.0327551936971984,296.223925943689,
-8.));
#11400=CARTESIAN_POINT('Ctrl Pts',(2.11083834575178,296.361425943689,-8.00877672769909));
#11401=CARTESIAN_POINT('Ctrl Pts',(3.97163317015235,296.498925943689,-6.94458082712411));
#11402=CARTESIAN_POINT('Ctrl Pts',(5.83242799455291,296.636425943689,-5.88038492654913));
#11403=CARTESIAN_POINT('Ctrl Pts',(6.91182563342691,296.773925943689,-4.02836682984766));
#11404=CARTESIAN_POINT('Ctrl Pts',(7.99122327230091,296.911425943689,-2.17634873314618));
#11405=CARTESIAN_POINT('Ctrl Pts',(8.,297.048925943689,-0.0327551936971989));
#11406=CARTESIAN_POINT('Ctrl Pts',(8.00877672769909,297.186425943689,2.11083834575178));
#11407=CARTESIAN_POINT('Ctrl Pts',(6.94458082712411,297.323925943689,3.97163317015235));
#11408=CARTESIAN_POINT('Ctrl Pts',(5.88038492654913,297.461425943689,5.83242799455291));
#11409=CARTESIAN_POINT('Ctrl Pts',(4.02836682984766,297.598925943689,6.91182563342691));
#11410=CARTESIAN_POINT('Ctrl Pts',(2.17634873314619,297.736425943689,7.99122327230091));
#11411=CARTESIAN_POINT('Ctrl Pts',(0.0327551936971994,297.873925943689,
8.));
#11412=CARTESIAN_POINT('Ctrl Pts',(-2.11083834575178,298.011425943689,8.00877672769909));
#11413=CARTESIAN_POINT('Ctrl Pts',(-3.97163317015234,298.148925943689,6.94458082712412));
#11414=CARTESIAN_POINT('Ctrl Pts',(-5.83242799455291,298.286425943689,5.88038492654913));
#11415=CARTESIAN_POINT('Ctrl Pts',(-6.91182563342691,298.423925943689,4.02836682984766));
#11416=CARTESIAN_POINT('Ctrl Pts',(-7.99122327230091,298.561425943689,2.17634873314619));
#11417=CARTESIAN_POINT('Ctrl Pts',(-8.,298.698925943689,0.0327551936971979));
#11418=CARTESIAN_POINT('Ctrl Pts',(-8.00877672769909,298.836425943689,-2.11083834575178));
#11419=CARTESIAN_POINT('Ctrl Pts',(-6.94458082712411,298.973925943689,-3.97163317015235));
#11420=CARTESIAN_POINT('Ctrl Pts',(-5.88038492654913,299.111425943689,-5.83242799455291));
#11421=CARTESIAN_POINT('Ctrl Pts',(-4.02836682984766,299.248925943689,-6.91182563342691));
#11422=CARTESIAN_POINT('Ctrl Pts',(-2.17634873314618,299.386425943689,-7.99122327230091));
#11423=CARTESIAN_POINT('Ctrl Pts',(-0.0327551936971984,299.523925943689,
-8.));
#11424=CARTESIAN_POINT('Ctrl Pts',(2.11083834575178,299.661425943689,-8.00877672769909));
#11425=CARTESIAN_POINT('Ctrl Pts',(3.97163317015235,299.798925943689,-6.94458082712411));
#11426=CARTESIAN_POINT('Ctrl Pts',(5.83242799455291,299.936425943689,-5.88038492654913));
#11427=CARTESIAN_POINT('Ctrl Pts',(6.91182563342691,300.073925943689,-4.02836682984766));
#11428=CARTESIAN_POINT('Ctrl Pts',(7.99122327230091,300.211425943689,-2.17634873314618));
#11429=CARTESIAN_POINT('Ctrl Pts',(8.,300.348925943689,-0.0327551936971989));
#11430=CARTESIAN_POINT('Ctrl Pts',(8.00877672769909,300.486425943689,2.11083834575178));
#11431=CARTESIAN_POINT('Ctrl Pts',(6.94458082712411,300.623925943689,3.97163317015235));
#11432=CARTESIAN_POINT('Ctrl Pts',(5.88038492654913,300.761425943689,5.83242799455291));
#11433=CARTESIAN_POINT('Ctrl Pts',(4.02836682984766,300.898925943689,6.91182563342691));
#11434=CARTESIAN_POINT('Ctrl Pts',(2.17634873314619,301.036425943689,7.99122327230091));
#11435=CARTESIAN_POINT('Ctrl Pts',(0.0327551936971994,301.173925943689,
8.));
#11436=CARTESIAN_POINT('Ctrl Pts',(-2.11083834575178,301.311425943689,8.00877672769909));
#11437=CARTESIAN_POINT('Ctrl Pts',(-3.97163317015234,301.448925943689,6.94458082712412));
#11438=CARTESIAN_POINT('Ctrl Pts',(-5.83242799455291,301.586425943689,5.88038492654913));
#11439=CARTESIAN_POINT('Ctrl Pts',(-6.91182563342691,301.723925943689,4.02836682984766));
#11440=CARTESIAN_POINT('Ctrl Pts',(-7.99122327230091,301.861425943689,2.17634873314619));
#11441=CARTESIAN_POINT('Ctrl Pts',(-8.,301.998925943689,0.0327551936971979));
#11442=CARTESIAN_POINT('Ctrl Pts',(-8.00877672769909,302.136425943689,-2.11083834575178));
#11443=CARTESIAN_POINT('Ctrl Pts',(-6.94458082712411,302.273925943689,-3.97163317015235));
#11444=CARTESIAN_POINT('Ctrl Pts',(-5.88038492654913,302.411425943689,-5.83242799455291));
#11445=CARTESIAN_POINT('Ctrl Pts',(-4.02836682984766,302.548925943689,-6.91182563342691));
#11446=CARTESIAN_POINT('Ctrl Pts',(-2.17634873314618,302.686425943689,-7.99122327230091));
#11447=CARTESIAN_POINT('Ctrl Pts',(-0.0327551936971984,302.823925943689,
-8.));
#11448=CARTESIAN_POINT('Ctrl Pts',(2.11083834575178,302.961425943689,-8.00877672769909));
#11449=CARTESIAN_POINT('Ctrl Pts',(3.97163317015235,303.098925943689,-6.94458082712411));
#11450=CARTESIAN_POINT('Ctrl Pts',(5.83242799455291,303.236425943689,-5.88038492654913));
#11451=CARTESIAN_POINT('Ctrl Pts',(6.91182563342691,303.373925943689,-4.02836682984766));
#11452=CARTESIAN_POINT('Ctrl Pts',(7.99122327230091,303.511425943689,-2.17634873314618));
#11453=CARTESIAN_POINT('Ctrl Pts',(8.,303.648925943689,-0.0327551936971989));
#11454=CARTESIAN_POINT('Ctrl Pts',(8.00877672769909,303.786425943689,2.11083834575178));
#11455=CARTESIAN_POINT('Ctrl Pts',(6.94458082712411,303.923925943689,3.97163317015235));
#11456=CARTESIAN_POINT('Ctrl Pts',(5.88038492654913,304.061425943689,5.83242799455291));
#11457=CARTESIAN_POINT('Ctrl Pts',(4.02836682984766,304.198925943689,6.91182563342691));
#11458=CARTESIAN_POINT('Ctrl Pts',(2.17634873314619,304.336425943689,7.99122327230091));
#11459=CARTESIAN_POINT('Ctrl Pts',(0.0327551936971994,304.473925943689,
8.));
#11460=CARTESIAN_POINT('Ctrl Pts',(-2.11083834575178,304.611425943689,8.00877672769909));
#11461=CARTESIAN_POINT('Ctrl Pts',(-3.97163317015234,304.748925943689,6.94458082712412));
#11462=CARTESIAN_POINT('Ctrl Pts',(-5.83242799455291,304.886425943689,5.88038492654913));
#11463=CARTESIAN_POINT('Ctrl Pts',(-6.91182563342691,305.023925943689,4.02836682984766));
#11464=CARTESIAN_POINT('Ctrl Pts',(-7.99122327230091,305.161425943689,2.17634873314619));
#11465=CARTESIAN_POINT('Ctrl Pts',(-8.,305.298925943689,0.0327551936971979));
#11466=CARTESIAN_POINT('Ctrl Pts',(-8.00877672769909,305.436425943689,-2.11083834575178));
#11467=CARTESIAN_POINT('Ctrl Pts',(-6.94458082712411,305.573925943689,-3.97163317015235));
#11468=CARTESIAN_POINT('Ctrl Pts',(-5.88038492654913,305.711425943689,-5.83242799455291));
#11469=CARTESIAN_POINT('Ctrl Pts',(-4.02836682984766,305.848925943689,-6.91182563342691));
#11470=CARTESIAN_POINT('Ctrl Pts',(-2.17634873314618,305.986425943689,-7.99122327230091));
#11471=CARTESIAN_POINT('Ctrl Pts',(-0.0327551936971984,306.123925943689,
-8.));
#11472=CARTESIAN_POINT('Ctrl Pts',(2.11083834575178,306.261425943689,-8.00877672769909));
#11473=CARTESIAN_POINT('Ctrl Pts',(3.97163317015235,306.398925943689,-6.94458082712411));
#11474=CARTESIAN_POINT('Ctrl Pts',(5.83242799455291,306.536425943689,-5.88038492654913));
#11475=CARTESIAN_POINT('Ctrl Pts',(6.91182563342691,306.673925943689,-4.02836682984766));
#11476=CARTESIAN_POINT('Ctrl Pts',(7.99122327230091,306.811425943689,-2.17634873314618));
#11477=CARTESIAN_POINT('Ctrl Pts',(8.,306.948925943689,-0.0327551936971989));
#11478=CARTESIAN_POINT('Ctrl Pts',(8.00877672769909,307.086425943689,2.11083834575178));
#11479=CARTESIAN_POINT('Ctrl Pts',(6.94458082712411,307.223925943689,3.97163317015235));
#11480=CARTESIAN_POINT('Ctrl Pts',(5.88038492654913,307.361425943689,5.83242799455291));
#11481=CARTESIAN_POINT('Ctrl Pts',(4.02836682984766,307.498925943689,6.91182563342691));
#11482=CARTESIAN_POINT('Ctrl Pts',(2.17634873314619,307.636425943689,7.99122327230091));
#11483=CARTESIAN_POINT('Ctrl Pts',(0.0327551936971994,307.773925943689,
8.));
#11484=CARTESIAN_POINT('Ctrl Pts',(-2.11083834575178,307.911425943689,8.00877672769909));
#11485=CARTESIAN_POINT('Ctrl Pts',(-3.97163317015234,308.048925943689,6.94458082712412));
#11486=CARTESIAN_POINT('Ctrl Pts',(-5.83242799455291,308.186425943689,5.88038492654913));
#11487=CARTESIAN_POINT('Ctrl Pts',(-6.91182563342691,308.323925943689,4.02836682984766));
#11488=CARTESIAN_POINT('Ctrl Pts',(-7.99122327230091,308.461425943689,2.17634873314619));
#11489=CARTESIAN_POINT('Ctrl Pts',(-8.,308.598925943689,0.0327551936971979));
#11490=CARTESIAN_POINT('Ctrl Pts',(-8.00877672769909,308.736425943689,-2.11083834575178));
#11491=CARTESIAN_POINT('Ctrl Pts',(-6.94458082712411,308.873925943689,-3.97163317015235));
#11492=CARTESIAN_POINT('Ctrl Pts',(-5.88038492654913,309.011425943689,-5.83242799455291));
#11493=CARTESIAN_POINT('Ctrl Pts',(-4.02836682984766,309.148925943689,-6.91182563342691));
#11494=CARTESIAN_POINT('Ctrl Pts',(-2.17634873314618,309.286425943689,-7.99122327230091));
#11495=CARTESIAN_POINT('Ctrl Pts',(-0.0327551936971984,309.423925943689,
-8.));
#11496=CARTESIAN_POINT('Ctrl Pts',(2.11083834575178,309.561425943689,-8.00877672769909));
#11497=CARTESIAN_POINT('Ctrl Pts',(3.97163317015235,309.698925943689,-6.94458082712411));
#11498=CARTESIAN_POINT('Ctrl Pts',(5.83242799455291,309.836425943689,-5.88038492654913));
#11499=CARTESIAN_POINT('Ctrl Pts',(6.91182563342691,309.973925943689,-4.02836682984766));
#11500=CARTESIAN_POINT('Ctrl Pts',(7.99122327230091,310.111425943689,-2.17634873314618));
#11501=CARTESIAN_POINT('Ctrl Pts',(8.,310.248925943689,-0.0327551936971989));
#11502=CARTESIAN_POINT('Ctrl Pts',(8.00877672769909,310.386425943689,2.11083834575178));
#11503=CARTESIAN_POINT('Ctrl Pts',(6.94458082712411,310.523925943689,3.97163317015235));
#11504=CARTESIAN_POINT('Ctrl Pts',(5.88038492654913,310.661425943689,5.83242799455291));
#11505=CARTESIAN_POINT('Ctrl Pts',(4.02836682984766,310.798925943689,6.91182563342691));
#11506=CARTESIAN_POINT('Ctrl Pts',(2.17634873314619,310.936425943689,7.99122327230091));
#11507=CARTESIAN_POINT('Ctrl Pts',(0.0327551936971994,311.073925943689,
8.));
#11508=CARTESIAN_POINT('Ctrl Pts',(-2.11083834575178,311.211425943689,8.00877672769909));
#11509=CARTESIAN_POINT('Ctrl Pts',(-3.97163317015234,311.348925943689,6.94458082712412));
#11510=CARTESIAN_POINT('Ctrl Pts',(-5.83242799455291,311.486425943689,5.88038492654913));
#11511=CARTESIAN_POINT('Ctrl Pts',(-6.91182563342691,311.623925943689,4.02836682984766));
#11512=CARTESIAN_POINT('Ctrl Pts',(-7.99122327230091,311.761425943689,2.17634873314619));
#11513=CARTESIAN_POINT('Ctrl Pts',(-8.,311.898925943689,0.0327551936971979));
#11514=CARTESIAN_POINT('Ctrl Pts',(-8.00877672769909,312.036425943689,-2.11083834575178));
#11515=CARTESIAN_POINT('Ctrl Pts',(-6.94458082712411,312.173925943689,-3.97163317015235));
#11516=CARTESIAN_POINT('Ctrl Pts',(-5.88038492654913,312.311425943689,-5.83242799455291));
#11517=CARTESIAN_POINT('Ctrl Pts',(-4.02836682984766,312.448925943689,-6.91182563342691));
#11518=CARTESIAN_POINT('Ctrl Pts',(-2.17634873314618,312.586425943689,-7.99122327230091));
#11519=CARTESIAN_POINT('Ctrl Pts',(-0.0327551936971984,312.723925943689,
-8.));
#11520=CARTESIAN_POINT('Ctrl Pts',(2.11083834575178,312.861425943689,-8.00877672769909));
#11521=CARTESIAN_POINT('Ctrl Pts',(3.97163317015235,312.998925943689,-6.94458082712411));
#11522=CARTESIAN_POINT('Ctrl Pts',(5.83242799455291,313.136425943689,-5.88038492654913));
#11523=CARTESIAN_POINT('Ctrl Pts',(6.91182563342691,313.273925943689,-4.02836682984766));
#11524=CARTESIAN_POINT('Ctrl Pts',(7.99122327230091,313.411425943689,-2.17634873314618));
#11525=CARTESIAN_POINT('Ctrl Pts',(8.,313.548925943689,-0.0327551936971989));
#11526=CARTESIAN_POINT('Ctrl Pts',(8.00877672769909,313.686425943689,2.11083834575178));
#11527=CARTESIAN_POINT('Ctrl Pts',(6.94458082712411,313.823925943689,3.97163317015235));
#11528=CARTESIAN_POINT('Ctrl Pts',(5.88038492654913,313.961425943689,5.83242799455291));
#11529=CARTESIAN_POINT('Ctrl Pts',(4.02836682984766,314.098925943689,6.91182563342691));
#11530=CARTESIAN_POINT('Ctrl Pts',(2.17634873314619,314.236425943689,7.99122327230091));
#11531=CARTESIAN_POINT('Ctrl Pts',(0.0327551936971994,314.373925943689,
8.));
#11532=CARTESIAN_POINT('Ctrl Pts',(-2.11083834575178,314.511425943689,8.00877672769909));
#11533=CARTESIAN_POINT('Ctrl Pts',(-3.97163317015234,314.648925943689,6.94458082712412));
#11534=CARTESIAN_POINT('Ctrl Pts',(-5.83242799455291,314.786425943689,5.88038492654913));
#11535=CARTESIAN_POINT('Ctrl Pts',(-6.91182563342691,314.923925943689,4.02836682984766));
#11536=CARTESIAN_POINT('Ctrl Pts',(-7.99122327230091,315.061425943689,2.17634873314619));
#11537=CARTESIAN_POINT('Ctrl Pts',(-8.,315.198925943689,0.0327551936971979));
#11538=CARTESIAN_POINT('Ctrl Pts',(-8.00877672769909,315.336425943689,-2.11083834575178));
#11539=CARTESIAN_POINT('Ctrl Pts',(-6.94458082712411,315.473925943689,-3.97163317015235));
#11540=CARTESIAN_POINT('Ctrl Pts',(-5.88038492654913,315.611425943689,-5.83242799455291));
#11541=CARTESIAN_POINT('Ctrl Pts',(-4.02836682984766,315.748925943689,-6.91182563342691));
#11542=CARTESIAN_POINT('Ctrl Pts',(-2.17634873314618,315.886425943689,-7.99122327230091));
#11543=CARTESIAN_POINT('Ctrl Pts',(-0.0327551936971984,316.023925943689,
-8.));
#11544=CARTESIAN_POINT('Ctrl Pts',(2.11083834575178,316.161425943689,-8.00877672769909));
#11545=CARTESIAN_POINT('Ctrl Pts',(3.97163317015235,316.298925943689,-6.94458082712411));
#11546=CARTESIAN_POINT('Ctrl Pts',(5.83242799455291,316.436425943689,-5.88038492654913));
#11547=CARTESIAN_POINT('Ctrl Pts',(6.91182563342691,316.573925943689,-4.02836682984766));
#11548=CARTESIAN_POINT('Ctrl Pts',(7.99122327230091,316.711425943689,-2.17634873314618));
#11549=CARTESIAN_POINT('Ctrl Pts',(8.,316.848925943689,-0.0327551936971989));
#11550=CARTESIAN_POINT('Ctrl Pts',(8.00877672769909,316.986425943689,2.11083834575178));
#11551=CARTESIAN_POINT('Ctrl Pts',(6.94458082712411,317.123925943689,3.97163317015235));
#11552=CARTESIAN_POINT('Ctrl Pts',(5.88038492654913,317.261425943689,5.83242799455291));
#11553=CARTESIAN_POINT('Ctrl Pts',(4.02836682984766,317.398925943689,6.91182563342691));
#11554=CARTESIAN_POINT('Ctrl Pts',(2.17634873314619,317.536425943689,7.99122327230091));
#11555=CARTESIAN_POINT('Ctrl Pts',(0.0327551936971994,317.673925943689,
8.));
#11556=CARTESIAN_POINT('Ctrl Pts',(-2.11083834575178,317.811425943689,8.00877672769909));
#11557=CARTESIAN_POINT('Ctrl Pts',(-3.97163317015234,317.948925943689,6.94458082712412));
#11558=CARTESIAN_POINT('Ctrl Pts',(-5.83242799455291,318.086425943689,5.88038492654913));
#11559=CARTESIAN_POINT('Ctrl Pts',(-6.91182563342691,318.223925943689,4.02836682984766));
#11560=CARTESIAN_POINT('Ctrl Pts',(-7.99122327230091,318.361425943689,2.17634873314619));
#11561=CARTESIAN_POINT('Ctrl Pts',(-8.,318.498925943689,0.0327551936971979));
#11562=CARTESIAN_POINT('Origin',(-8.,285.,8.32667268468867E-14));
#11563=CARTESIAN_POINT('Origin',(-8.,284.501074056311,-0.0327551936970314));
#11564=CARTESIAN_POINT('',(-8.49999999999999,285.,8.09585094317261E-14));
#11565=CARTESIAN_POINT('Origin',(-8.,285.,8.32667268468867E-14));
#11566=CARTESIAN_POINT('',(-8.,285.,7.59754672369217E-14));
#11567=CARTESIAN_POINT('Ctrl Pts',(-8.,285.498925943689,0.0327551936971979));
#11568=CARTESIAN_POINT('Ctrl Pts',(-8.00877672769909,285.636425943689,-2.11083834575178));
#11569=CARTESIAN_POINT('Ctrl Pts',(-6.94458082712411,285.773925943689,-3.97163317015235));
#11570=CARTESIAN_POINT('Ctrl Pts',(-5.88038492654913,285.911425943689,-5.83242799455291));
#11571=CARTESIAN_POINT('Ctrl Pts',(-4.02836682984766,286.048925943689,-6.91182563342691));
#11572=CARTESIAN_POINT('Ctrl Pts',(-2.17634873314618,286.186425943689,-7.99122327230091));
#11573=CARTESIAN_POINT('Ctrl Pts',(-0.0327551936971984,286.323925943689,
-8.));
#11574=CARTESIAN_POINT('Ctrl Pts',(2.11083834575178,286.461425943689,-8.00877672769909));
#11575=CARTESIAN_POINT('Ctrl Pts',(3.97163317015235,286.598925943689,-6.94458082712411));
#11576=CARTESIAN_POINT('Ctrl Pts',(5.83242799455291,286.736425943689,-5.88038492654913));
#11577=CARTESIAN_POINT('Ctrl Pts',(6.91182563342691,286.873925943689,-4.02836682984766));
#11578=CARTESIAN_POINT('Ctrl Pts',(7.99122327230091,287.011425943689,-2.17634873314618));
#11579=CARTESIAN_POINT('Ctrl Pts',(8.,287.148925943689,-0.0327551936971989));
#11580=CARTESIAN_POINT('Ctrl Pts',(8.00877672769909,287.286425943689,2.11083834575178));
#11581=CARTESIAN_POINT('Ctrl Pts',(6.94458082712411,287.423925943689,3.97163317015235));
#11582=CARTESIAN_POINT('Ctrl Pts',(5.88038492654913,287.561425943689,5.83242799455291));
#11583=CARTESIAN_POINT('Ctrl Pts',(4.02836682984766,287.698925943689,6.91182563342691));
#11584=CARTESIAN_POINT('Ctrl Pts',(2.17634873314619,287.836425943689,7.99122327230091));
#11585=CARTESIAN_POINT('Ctrl Pts',(0.0327551936971994,287.973925943689,
8.));
#11586=CARTESIAN_POINT('Ctrl Pts',(-2.11083834575178,288.111425943689,8.00877672769909));
#11587=CARTESIAN_POINT('Ctrl Pts',(-3.97163317015234,288.248925943689,6.94458082712412));
#11588=CARTESIAN_POINT('Ctrl Pts',(-5.83242799455291,288.386425943689,5.88038492654913));
#11589=CARTESIAN_POINT('Ctrl Pts',(-6.91182563342691,288.523925943689,4.02836682984766));
#11590=CARTESIAN_POINT('Ctrl Pts',(-7.99122327230091,288.661425943689,2.17634873314619));
#11591=CARTESIAN_POINT('Ctrl Pts',(-8.,288.798925943689,0.0327551936971979));
#11592=CARTESIAN_POINT('Ctrl Pts',(-8.00877672769909,288.936425943689,-2.11083834575178));
#11593=CARTESIAN_POINT('Ctrl Pts',(-6.94458082712411,289.073925943689,-3.97163317015235));
#11594=CARTESIAN_POINT('Ctrl Pts',(-5.88038492654913,289.211425943689,-5.83242799455291));
#11595=CARTESIAN_POINT('Ctrl Pts',(-4.02836682984766,289.348925943689,-6.91182563342691));
#11596=CARTESIAN_POINT('Ctrl Pts',(-2.17634873314618,289.486425943689,-7.99122327230091));
#11597=CARTESIAN_POINT('Ctrl Pts',(-0.0327551936971984,289.623925943689,
-8.));
#11598=CARTESIAN_POINT('Ctrl Pts',(2.11083834575178,289.761425943689,-8.00877672769909));
#11599=CARTESIAN_POINT('Ctrl Pts',(3.97163317015235,289.898925943689,-6.94458082712411));
#11600=CARTESIAN_POINT('Ctrl Pts',(5.83242799455291,290.036425943689,-5.88038492654913));
#11601=CARTESIAN_POINT('Ctrl Pts',(6.91182563342691,290.173925943689,-4.02836682984766));
#11602=CARTESIAN_POINT('Ctrl Pts',(7.99122327230091,290.311425943689,-2.17634873314618));
#11603=CARTESIAN_POINT('Ctrl Pts',(8.,290.448925943689,-0.0327551936971989));
#11604=CARTESIAN_POINT('Ctrl Pts',(8.00877672769909,290.586425943689,2.11083834575178));
#11605=CARTESIAN_POINT('Ctrl Pts',(6.94458082712411,290.723925943689,3.97163317015235));
#11606=CARTESIAN_POINT('Ctrl Pts',(5.88038492654913,290.861425943689,5.83242799455291));
#11607=CARTESIAN_POINT('Ctrl Pts',(4.02836682984766,290.998925943689,6.91182563342691));
#11608=CARTESIAN_POINT('Ctrl Pts',(2.17634873314619,291.136425943689,7.99122327230091));
#11609=CARTESIAN_POINT('Ctrl Pts',(0.0327551936971994,291.273925943689,
8.));
#11610=CARTESIAN_POINT('Ctrl Pts',(-2.11083834575178,291.411425943689,8.00877672769909));
#11611=CARTESIAN_POINT('Ctrl Pts',(-3.97163317015234,291.548925943689,6.94458082712412));
#11612=CARTESIAN_POINT('Ctrl Pts',(-5.83242799455291,291.686425943689,5.88038492654913));
#11613=CARTESIAN_POINT('Ctrl Pts',(-6.91182563342691,291.823925943689,4.02836682984766));
#11614=CARTESIAN_POINT('Ctrl Pts',(-7.99122327230091,291.961425943689,2.17634873314619));
#11615=CARTESIAN_POINT('Ctrl Pts',(-8.,292.098925943689,0.0327551936971979));
#11616=CARTESIAN_POINT('Ctrl Pts',(-8.00877672769909,292.236425943689,-2.11083834575178));
#11617=CARTESIAN_POINT('Ctrl Pts',(-6.94458082712411,292.373925943689,-3.97163317015235));
#11618=CARTESIAN_POINT('Ctrl Pts',(-5.88038492654913,292.511425943689,-5.83242799455291));
#11619=CARTESIAN_POINT('Ctrl Pts',(-4.02836682984766,292.648925943689,-6.91182563342691));
#11620=CARTESIAN_POINT('Ctrl Pts',(-2.17634873314618,292.786425943689,-7.99122327230091));
#11621=CARTESIAN_POINT('Ctrl Pts',(-0.0327551936971984,292.923925943689,
-8.));
#11622=CARTESIAN_POINT('Ctrl Pts',(2.11083834575178,293.061425943689,-8.00877672769909));
#11623=CARTESIAN_POINT('Ctrl Pts',(3.97163317015235,293.198925943689,-6.94458082712411));
#11624=CARTESIAN_POINT('Ctrl Pts',(5.83242799455291,293.336425943689,-5.88038492654913));
#11625=CARTESIAN_POINT('Ctrl Pts',(6.91182563342691,293.473925943689,-4.02836682984766));
#11626=CARTESIAN_POINT('Ctrl Pts',(7.99122327230091,293.611425943689,-2.17634873314618));
#11627=CARTESIAN_POINT('Ctrl Pts',(8.,293.748925943689,-0.0327551936971989));
#11628=CARTESIAN_POINT('Ctrl Pts',(8.00877672769909,293.886425943689,2.11083834575178));
#11629=CARTESIAN_POINT('Ctrl Pts',(6.94458082712411,294.023925943689,3.97163317015235));
#11630=CARTESIAN_POINT('Ctrl Pts',(5.88038492654913,294.161425943689,5.83242799455291));
#11631=CARTESIAN_POINT('Ctrl Pts',(4.02836682984766,294.298925943689,6.91182563342691));
#11632=CARTESIAN_POINT('Ctrl Pts',(2.17634873314619,294.436425943689,7.99122327230091));
#11633=CARTESIAN_POINT('Ctrl Pts',(0.0327551936971994,294.573925943689,
8.));
#11634=CARTESIAN_POINT('Ctrl Pts',(-2.11083834575178,294.711425943689,8.00877672769909));
#11635=CARTESIAN_POINT('Ctrl Pts',(-3.97163317015234,294.848925943689,6.94458082712412));
#11636=CARTESIAN_POINT('Ctrl Pts',(-5.83242799455291,294.986425943689,5.88038492654913));
#11637=CARTESIAN_POINT('Ctrl Pts',(-6.91182563342691,295.123925943689,4.02836682984766));
#11638=CARTESIAN_POINT('Ctrl Pts',(-7.99122327230091,295.261425943689,2.17634873314619));
#11639=CARTESIAN_POINT('Ctrl Pts',(-8.,295.398925943689,0.0327551936971979));
#11640=CARTESIAN_POINT('Ctrl Pts',(-8.00877672769909,295.536425943689,-2.11083834575178));
#11641=CARTESIAN_POINT('Ctrl Pts',(-6.94458082712411,295.673925943689,-3.97163317015235));
#11642=CARTESIAN_POINT('Ctrl Pts',(-5.88038492654913,295.811425943689,-5.83242799455291));
#11643=CARTESIAN_POINT('Ctrl Pts',(-4.02836682984766,295.948925943689,-6.91182563342691));
#11644=CARTESIAN_POINT('Ctrl Pts',(-2.17634873314618,296.086425943689,-7.99122327230091));
#11645=CARTESIAN_POINT('Ctrl Pts',(-0.0327551936971984,296.223925943689,
-8.));
#11646=CARTESIAN_POINT('Ctrl Pts',(2.11083834575178,296.361425943689,-8.00877672769909));
#11647=CARTESIAN_POINT('Ctrl Pts',(3.97163317015235,296.498925943689,-6.94458082712411));
#11648=CARTESIAN_POINT('Ctrl Pts',(5.83242799455291,296.636425943689,-5.88038492654913));
#11649=CARTESIAN_POINT('Ctrl Pts',(6.91182563342691,296.773925943689,-4.02836682984766));
#11650=CARTESIAN_POINT('Ctrl Pts',(7.99122327230091,296.911425943689,-2.17634873314618));
#11651=CARTESIAN_POINT('Ctrl Pts',(8.,297.048925943689,-0.0327551936971989));
#11652=CARTESIAN_POINT('Ctrl Pts',(8.00877672769909,297.186425943689,2.11083834575178));
#11653=CARTESIAN_POINT('Ctrl Pts',(6.94458082712411,297.323925943689,3.97163317015235));
#11654=CARTESIAN_POINT('Ctrl Pts',(5.88038492654913,297.461425943689,5.83242799455291));
#11655=CARTESIAN_POINT('Ctrl Pts',(4.02836682984766,297.598925943689,6.91182563342691));
#11656=CARTESIAN_POINT('Ctrl Pts',(2.17634873314619,297.736425943689,7.99122327230091));
#11657=CARTESIAN_POINT('Ctrl Pts',(0.0327551936971994,297.873925943689,
8.));
#11658=CARTESIAN_POINT('Ctrl Pts',(-2.11083834575178,298.011425943689,8.00877672769909));
#11659=CARTESIAN_POINT('Ctrl Pts',(-3.97163317015234,298.148925943689,6.94458082712412));
#11660=CARTESIAN_POINT('Ctrl Pts',(-5.83242799455291,298.286425943689,5.88038492654913));
#11661=CARTESIAN_POINT('Ctrl Pts',(-6.91182563342691,298.423925943689,4.02836682984766));
#11662=CARTESIAN_POINT('Ctrl Pts',(-7.99122327230091,298.561425943689,2.17634873314619));
#11663=CARTESIAN_POINT('Ctrl Pts',(-8.,298.698925943689,0.0327551936971979));
#11664=CARTESIAN_POINT('Ctrl Pts',(-8.00877672769909,298.836425943689,-2.11083834575178));
#11665=CARTESIAN_POINT('Ctrl Pts',(-6.94458082712411,298.973925943689,-3.97163317015235));
#11666=CARTESIAN_POINT('Ctrl Pts',(-5.88038492654913,299.111425943689,-5.83242799455291));
#11667=CARTESIAN_POINT('Ctrl Pts',(-4.02836682984766,299.248925943689,-6.91182563342691));
#11668=CARTESIAN_POINT('Ctrl Pts',(-2.17634873314618,299.386425943689,-7.99122327230091));
#11669=CARTESIAN_POINT('Ctrl Pts',(-0.0327551936971984,299.523925943689,
-8.));
#11670=CARTESIAN_POINT('Ctrl Pts',(2.11083834575178,299.661425943689,-8.00877672769909));
#11671=CARTESIAN_POINT('Ctrl Pts',(3.97163317015235,299.798925943689,-6.94458082712411));
#11672=CARTESIAN_POINT('Ctrl Pts',(5.83242799455291,299.936425943689,-5.88038492654913));
#11673=CARTESIAN_POINT('Ctrl Pts',(6.91182563342691,300.073925943689,-4.02836682984766));
#11674=CARTESIAN_POINT('Ctrl Pts',(7.99122327230091,300.211425943689,-2.17634873314618));
#11675=CARTESIAN_POINT('Ctrl Pts',(8.,300.348925943689,-0.0327551936971989));
#11676=CARTESIAN_POINT('Ctrl Pts',(8.00877672769909,300.486425943689,2.11083834575178));
#11677=CARTESIAN_POINT('Ctrl Pts',(6.94458082712411,300.623925943689,3.97163317015235));
#11678=CARTESIAN_POINT('Ctrl Pts',(5.88038492654913,300.761425943689,5.83242799455291));
#11679=CARTESIAN_POINT('Ctrl Pts',(4.02836682984766,300.898925943689,6.91182563342691));
#11680=CARTESIAN_POINT('Ctrl Pts',(2.17634873314619,301.036425943689,7.99122327230091));
#11681=CARTESIAN_POINT('Ctrl Pts',(0.0327551936971994,301.173925943689,
8.));
#11682=CARTESIAN_POINT('Ctrl Pts',(-2.11083834575178,301.311425943689,8.00877672769909));
#11683=CARTESIAN_POINT('Ctrl Pts',(-3.97163317015234,301.448925943689,6.94458082712412));
#11684=CARTESIAN_POINT('Ctrl Pts',(-5.83242799455291,301.586425943689,5.88038492654913));
#11685=CARTESIAN_POINT('Ctrl Pts',(-6.91182563342691,301.723925943689,4.02836682984766));
#11686=CARTESIAN_POINT('Ctrl Pts',(-7.99122327230091,301.861425943689,2.17634873314619));
#11687=CARTESIAN_POINT('Ctrl Pts',(-8.,301.998925943689,0.0327551936971979));
#11688=CARTESIAN_POINT('Ctrl Pts',(-8.00877672769909,302.136425943689,-2.11083834575178));
#11689=CARTESIAN_POINT('Ctrl Pts',(-6.94458082712411,302.273925943689,-3.97163317015235));
#11690=CARTESIAN_POINT('Ctrl Pts',(-5.88038492654913,302.411425943689,-5.83242799455291));
#11691=CARTESIAN_POINT('Ctrl Pts',(-4.02836682984766,302.548925943689,-6.91182563342691));
#11692=CARTESIAN_POINT('Ctrl Pts',(-2.17634873314618,302.686425943689,-7.99122327230091));
#11693=CARTESIAN_POINT('Ctrl Pts',(-0.0327551936971984,302.823925943689,
-8.));
#11694=CARTESIAN_POINT('Ctrl Pts',(2.11083834575178,302.961425943689,-8.00877672769909));
#11695=CARTESIAN_POINT('Ctrl Pts',(3.97163317015235,303.098925943689,-6.94458082712411));
#11696=CARTESIAN_POINT('Ctrl Pts',(5.83242799455291,303.236425943689,-5.88038492654913));
#11697=CARTESIAN_POINT('Ctrl Pts',(6.91182563342691,303.373925943689,-4.02836682984766));
#11698=CARTESIAN_POINT('Ctrl Pts',(7.99122327230091,303.511425943689,-2.17634873314618));
#11699=CARTESIAN_POINT('Ctrl Pts',(8.,303.648925943689,-0.0327551936971989));
#11700=CARTESIAN_POINT('Ctrl Pts',(8.00877672769909,303.786425943689,2.11083834575178));
#11701=CARTESIAN_POINT('Ctrl Pts',(6.94458082712411,303.923925943689,3.97163317015235));
#11702=CARTESIAN_POINT('Ctrl Pts',(5.88038492654913,304.061425943689,5.83242799455291));
#11703=CARTESIAN_POINT('Ctrl Pts',(4.02836682984766,304.198925943689,6.91182563342691));
#11704=CARTESIAN_POINT('Ctrl Pts',(2.17634873314619,304.336425943689,7.99122327230091));
#11705=CARTESIAN_POINT('Ctrl Pts',(0.0327551936971994,304.473925943689,
8.));
#11706=CARTESIAN_POINT('Ctrl Pts',(-2.11083834575178,304.611425943689,8.00877672769909));
#11707=CARTESIAN_POINT('Ctrl Pts',(-3.97163317015234,304.748925943689,6.94458082712412));
#11708=CARTESIAN_POINT('Ctrl Pts',(-5.83242799455291,304.886425943689,5.88038492654913));
#11709=CARTESIAN_POINT('Ctrl Pts',(-6.91182563342691,305.023925943689,4.02836682984766));
#11710=CARTESIAN_POINT('Ctrl Pts',(-7.99122327230091,305.161425943689,2.17634873314619));
#11711=CARTESIAN_POINT('Ctrl Pts',(-8.,305.298925943689,0.0327551936971979));
#11712=CARTESIAN_POINT('Ctrl Pts',(-8.00877672769909,305.436425943689,-2.11083834575178));
#11713=CARTESIAN_POINT('Ctrl Pts',(-6.94458082712411,305.573925943689,-3.97163317015235));
#11714=CARTESIAN_POINT('Ctrl Pts',(-5.88038492654913,305.711425943689,-5.83242799455291));
#11715=CARTESIAN_POINT('Ctrl Pts',(-4.02836682984766,305.848925943689,-6.91182563342691));
#11716=CARTESIAN_POINT('Ctrl Pts',(-2.17634873314618,305.986425943689,-7.99122327230091));
#11717=CARTESIAN_POINT('Ctrl Pts',(-0.0327551936971984,306.123925943689,
-8.));
#11718=CARTESIAN_POINT('Ctrl Pts',(2.11083834575178,306.261425943689,-8.00877672769909));
#11719=CARTESIAN_POINT('Ctrl Pts',(3.97163317015235,306.398925943689,-6.94458082712411));
#11720=CARTESIAN_POINT('Ctrl Pts',(5.83242799455291,306.536425943689,-5.88038492654913));
#11721=CARTESIAN_POINT('Ctrl Pts',(6.91182563342691,306.673925943689,-4.02836682984766));
#11722=CARTESIAN_POINT('Ctrl Pts',(7.99122327230091,306.811425943689,-2.17634873314618));
#11723=CARTESIAN_POINT('Ctrl Pts',(8.,306.948925943689,-0.0327551936971989));
#11724=CARTESIAN_POINT('Ctrl Pts',(8.00877672769909,307.086425943689,2.11083834575178));
#11725=CARTESIAN_POINT('Ctrl Pts',(6.94458082712411,307.223925943689,3.97163317015235));
#11726=CARTESIAN_POINT('Ctrl Pts',(5.88038492654913,307.361425943689,5.83242799455291));
#11727=CARTESIAN_POINT('Ctrl Pts',(4.02836682984766,307.498925943689,6.91182563342691));
#11728=CARTESIAN_POINT('Ctrl Pts',(2.17634873314619,307.636425943689,7.99122327230091));
#11729=CARTESIAN_POINT('Ctrl Pts',(0.0327551936971994,307.773925943689,
8.));
#11730=CARTESIAN_POINT('Ctrl Pts',(-2.11083834575178,307.911425943689,8.00877672769909));
#11731=CARTESIAN_POINT('Ctrl Pts',(-3.97163317015234,308.048925943689,6.94458082712412));
#11732=CARTESIAN_POINT('Ctrl Pts',(-5.83242799455291,308.186425943689,5.88038492654913));
#11733=CARTESIAN_POINT('Ctrl Pts',(-6.91182563342691,308.323925943689,4.02836682984766));
#11734=CARTESIAN_POINT('Ctrl Pts',(-7.99122327230091,308.461425943689,2.17634873314619));
#11735=CARTESIAN_POINT('Ctrl Pts',(-8.,308.598925943689,0.0327551936971979));
#11736=CARTESIAN_POINT('Ctrl Pts',(-8.00877672769909,308.736425943689,-2.11083834575178));
#11737=CARTESIAN_POINT('Ctrl Pts',(-6.94458082712411,308.873925943689,-3.97163317015235));
#11738=CARTESIAN_POINT('Ctrl Pts',(-5.88038492654913,309.011425943689,-5.83242799455291));
#11739=CARTESIAN_POINT('Ctrl Pts',(-4.02836682984766,309.148925943689,-6.91182563342691));
#11740=CARTESIAN_POINT('Ctrl Pts',(-2.17634873314618,309.286425943689,-7.99122327230091));
#11741=CARTESIAN_POINT('Ctrl Pts',(-0.0327551936971984,309.423925943689,
-8.));
#11742=CARTESIAN_POINT('Ctrl Pts',(2.11083834575178,309.561425943689,-8.00877672769909));
#11743=CARTESIAN_POINT('Ctrl Pts',(3.97163317015235,309.698925943689,-6.94458082712411));
#11744=CARTESIAN_POINT('Ctrl Pts',(5.83242799455291,309.836425943689,-5.88038492654913));
#11745=CARTESIAN_POINT('Ctrl Pts',(6.91182563342691,309.973925943689,-4.02836682984766));
#11746=CARTESIAN_POINT('Ctrl Pts',(7.99122327230091,310.111425943689,-2.17634873314618));
#11747=CARTESIAN_POINT('Ctrl Pts',(8.,310.248925943689,-0.0327551936971989));
#11748=CARTESIAN_POINT('Ctrl Pts',(8.00877672769909,310.386425943689,2.11083834575178));
#11749=CARTESIAN_POINT('Ctrl Pts',(6.94458082712411,310.523925943689,3.97163317015235));
#11750=CARTESIAN_POINT('Ctrl Pts',(5.88038492654913,310.661425943689,5.83242799455291));
#11751=CARTESIAN_POINT('Ctrl Pts',(4.02836682984766,310.798925943689,6.91182563342691));
#11752=CARTESIAN_POINT('Ctrl Pts',(2.17634873314619,310.936425943689,7.99122327230091));
#11753=CARTESIAN_POINT('Ctrl Pts',(0.0327551936971994,311.073925943689,
8.));
#11754=CARTESIAN_POINT('Ctrl Pts',(-2.11083834575178,311.211425943689,8.00877672769909));
#11755=CARTESIAN_POINT('Ctrl Pts',(-3.97163317015234,311.348925943689,6.94458082712412));
#11756=CARTESIAN_POINT('Ctrl Pts',(-5.83242799455291,311.486425943689,5.88038492654913));
#11757=CARTESIAN_POINT('Ctrl Pts',(-6.91182563342691,311.623925943689,4.02836682984766));
#11758=CARTESIAN_POINT('Ctrl Pts',(-7.99122327230091,311.761425943689,2.17634873314619));
#11759=CARTESIAN_POINT('Ctrl Pts',(-8.,311.898925943689,0.0327551936971979));
#11760=CARTESIAN_POINT('Ctrl Pts',(-8.00877672769909,312.036425943689,-2.11083834575178));
#11761=CARTESIAN_POINT('Ctrl Pts',(-6.94458082712411,312.173925943689,-3.97163317015235));
#11762=CARTESIAN_POINT('Ctrl Pts',(-5.88038492654913,312.311425943689,-5.83242799455291));
#11763=CARTESIAN_POINT('Ctrl Pts',(-4.02836682984766,312.448925943689,-6.91182563342691));
#11764=CARTESIAN_POINT('Ctrl Pts',(-2.17634873314618,312.586425943689,-7.99122327230091));
#11765=CARTESIAN_POINT('Ctrl Pts',(-0.0327551936971984,312.723925943689,
-8.));
#11766=CARTESIAN_POINT('Ctrl Pts',(2.11083834575178,312.861425943689,-8.00877672769909));
#11767=CARTESIAN_POINT('Ctrl Pts',(3.97163317015235,312.998925943689,-6.94458082712411));
#11768=CARTESIAN_POINT('Ctrl Pts',(5.83242799455291,313.136425943689,-5.88038492654913));
#11769=CARTESIAN_POINT('Ctrl Pts',(6.91182563342691,313.273925943689,-4.02836682984766));
#11770=CARTESIAN_POINT('Ctrl Pts',(7.99122327230091,313.411425943689,-2.17634873314618));
#11771=CARTESIAN_POINT('Ctrl Pts',(8.,313.548925943689,-0.0327551936971989));
#11772=CARTESIAN_POINT('Ctrl Pts',(8.00877672769909,313.686425943689,2.11083834575178));
#11773=CARTESIAN_POINT('Ctrl Pts',(6.94458082712411,313.823925943689,3.97163317015235));
#11774=CARTESIAN_POINT('Ctrl Pts',(5.88038492654913,313.961425943689,5.83242799455291));
#11775=CARTESIAN_POINT('Ctrl Pts',(4.02836682984766,314.098925943689,6.91182563342691));
#11776=CARTESIAN_POINT('Ctrl Pts',(2.17634873314619,314.236425943689,7.99122327230091));
#11777=CARTESIAN_POINT('Ctrl Pts',(0.0327551936971994,314.373925943689,
8.));
#11778=CARTESIAN_POINT('Ctrl Pts',(-2.11083834575178,314.511425943689,8.00877672769909));
#11779=CARTESIAN_POINT('Ctrl Pts',(-3.97163317015234,314.648925943689,6.94458082712412));
#11780=CARTESIAN_POINT('Ctrl Pts',(-5.83242799455291,314.786425943689,5.88038492654913));
#11781=CARTESIAN_POINT('Ctrl Pts',(-6.91182563342691,314.923925943689,4.02836682984766));
#11782=CARTESIAN_POINT('Ctrl Pts',(-7.99122327230091,315.061425943689,2.17634873314619));
#11783=CARTESIAN_POINT('Ctrl Pts',(-8.,315.198925943689,0.0327551936971979));
#11784=CARTESIAN_POINT('Ctrl Pts',(-8.00877672769909,315.336425943689,-2.11083834575178));
#11785=CARTESIAN_POINT('Ctrl Pts',(-6.94458082712411,315.473925943689,-3.97163317015235));
#11786=CARTESIAN_POINT('Ctrl Pts',(-5.88038492654913,315.611425943689,-5.83242799455291));
#11787=CARTESIAN_POINT('Ctrl Pts',(-4.02836682984766,315.748925943689,-6.91182563342691));
#11788=CARTESIAN_POINT('Ctrl Pts',(-2.17634873314618,315.886425943689,-7.99122327230091));
#11789=CARTESIAN_POINT('Ctrl Pts',(-0.0327551936971984,316.023925943689,
-8.));
#11790=CARTESIAN_POINT('Ctrl Pts',(2.11083834575178,316.161425943689,-8.00877672769909));
#11791=CARTESIAN_POINT('Ctrl Pts',(3.97163317015235,316.298925943689,-6.94458082712411));
#11792=CARTESIAN_POINT('Ctrl Pts',(5.83242799455291,316.436425943689,-5.88038492654913));
#11793=CARTESIAN_POINT('Ctrl Pts',(6.91182563342691,316.573925943689,-4.02836682984766));
#11794=CARTESIAN_POINT('Ctrl Pts',(7.99122327230091,316.711425943689,-2.17634873314618));
#11795=CARTESIAN_POINT('Ctrl Pts',(8.,316.848925943689,-0.0327551936971989));
#11796=CARTESIAN_POINT('Ctrl Pts',(8.00877672769909,316.986425943689,2.11083834575178));
#11797=CARTESIAN_POINT('Ctrl Pts',(6.94458082712411,317.123925943689,3.97163317015235));
#11798=CARTESIAN_POINT('Ctrl Pts',(5.88038492654913,317.261425943689,5.83242799455291));
#11799=CARTESIAN_POINT('Ctrl Pts',(4.02836682984766,317.398925943689,6.91182563342691));
#11800=CARTESIAN_POINT('Ctrl Pts',(2.17634873314619,317.536425943689,7.99122327230091));
#11801=CARTESIAN_POINT('Ctrl Pts',(0.0327551936971994,317.673925943689,
8.));
#11802=CARTESIAN_POINT('Ctrl Pts',(-2.11083834575178,317.811425943689,8.00877672769909));
#11803=CARTESIAN_POINT('Ctrl Pts',(-3.97163317015234,317.948925943689,6.94458082712412));
#11804=CARTESIAN_POINT('Ctrl Pts',(-5.83242799455291,318.086425943689,5.88038492654913));
#11805=CARTESIAN_POINT('Ctrl Pts',(-6.91182563342691,318.223925943689,4.02836682984766));
#11806=CARTESIAN_POINT('Ctrl Pts',(-7.99122327230091,318.361425943689,2.17634873314619));
#11807=CARTESIAN_POINT('Ctrl Pts',(-8.,318.498925943689,0.0327551936971979));
#11808=CARTESIAN_POINT('Ctrl Pts',(-7.,285.498925943689,0.0327551936971879));
#11809=CARTESIAN_POINT('Ctrl Pts',(-7.00877672769909,285.636425943689,-1.84288915332067));
#11810=CARTESIAN_POINT('Ctrl Pts',(-6.07855542333967,285.773925943689,-3.47163317015236));
#11811=CARTESIAN_POINT('Ctrl Pts',(-5.14833411898024,285.911425943689,-5.10037718698404));
#11812=CARTESIAN_POINT('Ctrl Pts',(-3.52836682984765,286.048925943689,-6.04580022964248));
#11813=CARTESIAN_POINT('Ctrl Pts',(-1.90839954071505,286.186425943689,-6.99122327230092));
#11814=CARTESIAN_POINT('Ctrl Pts',(-0.0327551936971884,286.323925943689,
-7.));
#11815=CARTESIAN_POINT('Ctrl Pts',(1.84288915332067,286.461425943689,-7.00877672769909));
#11816=CARTESIAN_POINT('Ctrl Pts',(3.47163317015236,286.598925943689,-6.07855542333967));
#11817=CARTESIAN_POINT('Ctrl Pts',(5.10037718698404,286.736425943689,-5.14833411898024));
#11818=CARTESIAN_POINT('Ctrl Pts',(6.04580022964248,286.873925943689,-3.52836682984765));
#11819=CARTESIAN_POINT('Ctrl Pts',(6.99122327230092,287.011425943689,-1.90839954071505));
#11820=CARTESIAN_POINT('Ctrl Pts',(7.,287.148925943689,-0.0327551936971888));
#11821=CARTESIAN_POINT('Ctrl Pts',(7.00877672769909,287.286425943689,1.84288915332067));
#11822=CARTESIAN_POINT('Ctrl Pts',(6.07855542333967,287.423925943689,3.47163317015236));
#11823=CARTESIAN_POINT('Ctrl Pts',(5.14833411898025,287.561425943689,5.10037718698404));
#11824=CARTESIAN_POINT('Ctrl Pts',(3.52836682984765,287.698925943689,6.04580022964248));
#11825=CARTESIAN_POINT('Ctrl Pts',(1.90839954071505,287.836425943689,6.99122327230091));
#11826=CARTESIAN_POINT('Ctrl Pts',(0.0327551936971892,287.973925943689,
7.));
#11827=CARTESIAN_POINT('Ctrl Pts',(-1.84288915332067,288.111425943689,7.00877672769909));
#11828=CARTESIAN_POINT('Ctrl Pts',(-3.47163317015235,288.248925943689,6.07855542333967));
#11829=CARTESIAN_POINT('Ctrl Pts',(-5.10037718698404,288.386425943689,5.14833411898025));
#11830=CARTESIAN_POINT('Ctrl Pts',(-6.04580022964248,288.523925943689,3.52836682984765));
#11831=CARTESIAN_POINT('Ctrl Pts',(-6.99122327230091,288.661425943689,1.90839954071505));
#11832=CARTESIAN_POINT('Ctrl Pts',(-7.,288.798925943689,0.0327551936971879));
#11833=CARTESIAN_POINT('Ctrl Pts',(-7.00877672769909,288.936425943689,-1.84288915332067));
#11834=CARTESIAN_POINT('Ctrl Pts',(-6.07855542333967,289.073925943689,-3.47163317015236));
#11835=CARTESIAN_POINT('Ctrl Pts',(-5.14833411898024,289.211425943689,-5.10037718698404));
#11836=CARTESIAN_POINT('Ctrl Pts',(-3.52836682984765,289.348925943689,-6.04580022964248));
#11837=CARTESIAN_POINT('Ctrl Pts',(-1.90839954071505,289.486425943689,-6.99122327230092));
#11838=CARTESIAN_POINT('Ctrl Pts',(-0.0327551936971884,289.623925943689,
-7.));
#11839=CARTESIAN_POINT('Ctrl Pts',(1.84288915332067,289.761425943689,-7.00877672769909));
#11840=CARTESIAN_POINT('Ctrl Pts',(3.47163317015236,289.898925943689,-6.07855542333967));
#11841=CARTESIAN_POINT('Ctrl Pts',(5.10037718698404,290.036425943689,-5.14833411898024));
#11842=CARTESIAN_POINT('Ctrl Pts',(6.04580022964248,290.173925943689,-3.52836682984765));
#11843=CARTESIAN_POINT('Ctrl Pts',(6.99122327230092,290.311425943689,-1.90839954071505));
#11844=CARTESIAN_POINT('Ctrl Pts',(7.,290.448925943689,-0.0327551936971888));
#11845=CARTESIAN_POINT('Ctrl Pts',(7.00877672769909,290.586425943689,1.84288915332067));
#11846=CARTESIAN_POINT('Ctrl Pts',(6.07855542333967,290.723925943689,3.47163317015236));
#11847=CARTESIAN_POINT('Ctrl Pts',(5.14833411898025,290.861425943689,5.10037718698404));
#11848=CARTESIAN_POINT('Ctrl Pts',(3.52836682984765,290.998925943689,6.04580022964248));
#11849=CARTESIAN_POINT('Ctrl Pts',(1.90839954071505,291.136425943689,6.99122327230091));
#11850=CARTESIAN_POINT('Ctrl Pts',(0.0327551936971892,291.273925943689,
7.));
#11851=CARTESIAN_POINT('Ctrl Pts',(-1.84288915332067,291.411425943689,7.00877672769909));
#11852=CARTESIAN_POINT('Ctrl Pts',(-3.47163317015235,291.548925943689,6.07855542333967));
#11853=CARTESIAN_POINT('Ctrl Pts',(-5.10037718698404,291.686425943689,5.14833411898025));
#11854=CARTESIAN_POINT('Ctrl Pts',(-6.04580022964248,291.823925943689,3.52836682984765));
#11855=CARTESIAN_POINT('Ctrl Pts',(-6.99122327230091,291.961425943689,1.90839954071505));
#11856=CARTESIAN_POINT('Ctrl Pts',(-7.,292.098925943689,0.0327551936971879));
#11857=CARTESIAN_POINT('Ctrl Pts',(-7.00877672769909,292.236425943689,-1.84288915332067));
#11858=CARTESIAN_POINT('Ctrl Pts',(-6.07855542333967,292.373925943689,-3.47163317015236));
#11859=CARTESIAN_POINT('Ctrl Pts',(-5.14833411898024,292.511425943689,-5.10037718698404));
#11860=CARTESIAN_POINT('Ctrl Pts',(-3.52836682984765,292.648925943689,-6.04580022964248));
#11861=CARTESIAN_POINT('Ctrl Pts',(-1.90839954071505,292.786425943689,-6.99122327230092));
#11862=CARTESIAN_POINT('Ctrl Pts',(-0.0327551936971884,292.923925943689,
-7.));
#11863=CARTESIAN_POINT('Ctrl Pts',(1.84288915332067,293.061425943689,-7.00877672769909));
#11864=CARTESIAN_POINT('Ctrl Pts',(3.47163317015236,293.198925943689,-6.07855542333967));
#11865=CARTESIAN_POINT('Ctrl Pts',(5.10037718698404,293.336425943689,-5.14833411898024));
#11866=CARTESIAN_POINT('Ctrl Pts',(6.04580022964248,293.473925943689,-3.52836682984765));
#11867=CARTESIAN_POINT('Ctrl Pts',(6.99122327230092,293.611425943689,-1.90839954071505));
#11868=CARTESIAN_POINT('Ctrl Pts',(7.,293.748925943689,-0.0327551936971888));
#11869=CARTESIAN_POINT('Ctrl Pts',(7.00877672769909,293.886425943689,1.84288915332067));
#11870=CARTESIAN_POINT('Ctrl Pts',(6.07855542333967,294.023925943689,3.47163317015236));
#11871=CARTESIAN_POINT('Ctrl Pts',(5.14833411898025,294.161425943689,5.10037718698404));
#11872=CARTESIAN_POINT('Ctrl Pts',(3.52836682984765,294.298925943689,6.04580022964248));
#11873=CARTESIAN_POINT('Ctrl Pts',(1.90839954071505,294.436425943689,6.99122327230091));
#11874=CARTESIAN_POINT('Ctrl Pts',(0.0327551936971892,294.573925943689,
7.));
#11875=CARTESIAN_POINT('Ctrl Pts',(-1.84288915332067,294.711425943689,7.00877672769909));
#11876=CARTESIAN_POINT('Ctrl Pts',(-3.47163317015235,294.848925943689,6.07855542333967));
#11877=CARTESIAN_POINT('Ctrl Pts',(-5.10037718698404,294.986425943689,5.14833411898025));
#11878=CARTESIAN_POINT('Ctrl Pts',(-6.04580022964248,295.123925943689,3.52836682984765));
#11879=CARTESIAN_POINT('Ctrl Pts',(-6.99122327230091,295.261425943689,1.90839954071505));
#11880=CARTESIAN_POINT('Ctrl Pts',(-7.,295.398925943689,0.0327551936971879));
#11881=CARTESIAN_POINT('Ctrl Pts',(-7.00877672769909,295.536425943689,-1.84288915332067));
#11882=CARTESIAN_POINT('Ctrl Pts',(-6.07855542333967,295.673925943689,-3.47163317015236));
#11883=CARTESIAN_POINT('Ctrl Pts',(-5.14833411898024,295.811425943689,-5.10037718698404));
#11884=CARTESIAN_POINT('Ctrl Pts',(-3.52836682984765,295.948925943689,-6.04580022964248));
#11885=CARTESIAN_POINT('Ctrl Pts',(-1.90839954071505,296.086425943689,-6.99122327230092));
#11886=CARTESIAN_POINT('Ctrl Pts',(-0.0327551936971884,296.223925943689,
-7.));
#11887=CARTESIAN_POINT('Ctrl Pts',(1.84288915332067,296.361425943689,-7.00877672769909));
#11888=CARTESIAN_POINT('Ctrl Pts',(3.47163317015236,296.498925943689,-6.07855542333967));
#11889=CARTESIAN_POINT('Ctrl Pts',(5.10037718698404,296.636425943689,-5.14833411898024));
#11890=CARTESIAN_POINT('Ctrl Pts',(6.04580022964248,296.773925943689,-3.52836682984765));
#11891=CARTESIAN_POINT('Ctrl Pts',(6.99122327230092,296.911425943689,-1.90839954071505));
#11892=CARTESIAN_POINT('Ctrl Pts',(7.,297.048925943689,-0.0327551936971888));
#11893=CARTESIAN_POINT('Ctrl Pts',(7.00877672769909,297.186425943689,1.84288915332067));
#11894=CARTESIAN_POINT('Ctrl Pts',(6.07855542333967,297.323925943689,3.47163317015236));
#11895=CARTESIAN_POINT('Ctrl Pts',(5.14833411898025,297.461425943689,5.10037718698404));
#11896=CARTESIAN_POINT('Ctrl Pts',(3.52836682984765,297.598925943689,6.04580022964248));
#11897=CARTESIAN_POINT('Ctrl Pts',(1.90839954071505,297.736425943689,6.99122327230091));
#11898=CARTESIAN_POINT('Ctrl Pts',(0.0327551936971892,297.873925943689,
7.));
#11899=CARTESIAN_POINT('Ctrl Pts',(-1.84288915332067,298.011425943689,7.00877672769909));
#11900=CARTESIAN_POINT('Ctrl Pts',(-3.47163317015235,298.148925943689,6.07855542333967));
#11901=CARTESIAN_POINT('Ctrl Pts',(-5.10037718698404,298.286425943689,5.14833411898025));
#11902=CARTESIAN_POINT('Ctrl Pts',(-6.04580022964248,298.423925943689,3.52836682984765));
#11903=CARTESIAN_POINT('Ctrl Pts',(-6.99122327230091,298.561425943689,1.90839954071505));
#11904=CARTESIAN_POINT('Ctrl Pts',(-7.,298.698925943689,0.0327551936971879));
#11905=CARTESIAN_POINT('Ctrl Pts',(-7.00877672769909,298.836425943689,-1.84288915332067));
#11906=CARTESIAN_POINT('Ctrl Pts',(-6.07855542333967,298.973925943689,-3.47163317015236));
#11907=CARTESIAN_POINT('Ctrl Pts',(-5.14833411898024,299.111425943689,-5.10037718698404));
#11908=CARTESIAN_POINT('Ctrl Pts',(-3.52836682984765,299.248925943689,-6.04580022964248));
#11909=CARTESIAN_POINT('Ctrl Pts',(-1.90839954071505,299.386425943689,-6.99122327230092));
#11910=CARTESIAN_POINT('Ctrl Pts',(-0.0327551936971884,299.523925943689,
-7.));
#11911=CARTESIAN_POINT('Ctrl Pts',(1.84288915332067,299.661425943689,-7.00877672769909));
#11912=CARTESIAN_POINT('Ctrl Pts',(3.47163317015236,299.798925943689,-6.07855542333967));
#11913=CARTESIAN_POINT('Ctrl Pts',(5.10037718698404,299.936425943689,-5.14833411898024));
#11914=CARTESIAN_POINT('Ctrl Pts',(6.04580022964248,300.073925943689,-3.52836682984765));
#11915=CARTESIAN_POINT('Ctrl Pts',(6.99122327230092,300.211425943689,-1.90839954071505));
#11916=CARTESIAN_POINT('Ctrl Pts',(7.,300.348925943689,-0.0327551936971888));
#11917=CARTESIAN_POINT('Ctrl Pts',(7.00877672769909,300.486425943689,1.84288915332067));
#11918=CARTESIAN_POINT('Ctrl Pts',(6.07855542333967,300.623925943689,3.47163317015236));
#11919=CARTESIAN_POINT('Ctrl Pts',(5.14833411898025,300.761425943689,5.10037718698404));
#11920=CARTESIAN_POINT('Ctrl Pts',(3.52836682984765,300.898925943689,6.04580022964248));
#11921=CARTESIAN_POINT('Ctrl Pts',(1.90839954071505,301.036425943689,6.99122327230091));
#11922=CARTESIAN_POINT('Ctrl Pts',(0.0327551936971892,301.173925943689,
7.));
#11923=CARTESIAN_POINT('Ctrl Pts',(-1.84288915332067,301.311425943689,7.00877672769909));
#11924=CARTESIAN_POINT('Ctrl Pts',(-3.47163317015235,301.448925943689,6.07855542333967));
#11925=CARTESIAN_POINT('Ctrl Pts',(-5.10037718698404,301.586425943689,5.14833411898025));
#11926=CARTESIAN_POINT('Ctrl Pts',(-6.04580022964248,301.723925943689,3.52836682984765));
#11927=CARTESIAN_POINT('Ctrl Pts',(-6.99122327230091,301.861425943689,1.90839954071505));
#11928=CARTESIAN_POINT('Ctrl Pts',(-7.,301.998925943689,0.0327551936971879));
#11929=CARTESIAN_POINT('Ctrl Pts',(-7.00877672769909,302.136425943689,-1.84288915332067));
#11930=CARTESIAN_POINT('Ctrl Pts',(-6.07855542333967,302.273925943689,-3.47163317015236));
#11931=CARTESIAN_POINT('Ctrl Pts',(-5.14833411898024,302.411425943689,-5.10037718698404));
#11932=CARTESIAN_POINT('Ctrl Pts',(-3.52836682984765,302.548925943689,-6.04580022964248));
#11933=CARTESIAN_POINT('Ctrl Pts',(-1.90839954071505,302.686425943689,-6.99122327230092));
#11934=CARTESIAN_POINT('Ctrl Pts',(-0.0327551936971884,302.823925943689,
-7.));
#11935=CARTESIAN_POINT('Ctrl Pts',(1.84288915332067,302.961425943689,-7.00877672769909));
#11936=CARTESIAN_POINT('Ctrl Pts',(3.47163317015236,303.098925943689,-6.07855542333967));
#11937=CARTESIAN_POINT('Ctrl Pts',(5.10037718698404,303.236425943689,-5.14833411898024));
#11938=CARTESIAN_POINT('Ctrl Pts',(6.04580022964248,303.373925943689,-3.52836682984765));
#11939=CARTESIAN_POINT('Ctrl Pts',(6.99122327230092,303.511425943689,-1.90839954071505));
#11940=CARTESIAN_POINT('Ctrl Pts',(7.,303.648925943689,-0.0327551936971888));
#11941=CARTESIAN_POINT('Ctrl Pts',(7.00877672769909,303.786425943689,1.84288915332067));
#11942=CARTESIAN_POINT('Ctrl Pts',(6.07855542333967,303.923925943689,3.47163317015236));
#11943=CARTESIAN_POINT('Ctrl Pts',(5.14833411898025,304.061425943689,5.10037718698404));
#11944=CARTESIAN_POINT('Ctrl Pts',(3.52836682984765,304.198925943689,6.04580022964248));
#11945=CARTESIAN_POINT('Ctrl Pts',(1.90839954071505,304.336425943689,6.99122327230091));
#11946=CARTESIAN_POINT('Ctrl Pts',(0.0327551936971892,304.473925943689,
7.));
#11947=CARTESIAN_POINT('Ctrl Pts',(-1.84288915332067,304.611425943689,7.00877672769909));
#11948=CARTESIAN_POINT('Ctrl Pts',(-3.47163317015235,304.748925943689,6.07855542333967));
#11949=CARTESIAN_POINT('Ctrl Pts',(-5.10037718698404,304.886425943689,5.14833411898025));
#11950=CARTESIAN_POINT('Ctrl Pts',(-6.04580022964248,305.023925943689,3.52836682984765));
#11951=CARTESIAN_POINT('Ctrl Pts',(-6.99122327230091,305.161425943689,1.90839954071505));
#11952=CARTESIAN_POINT('Ctrl Pts',(-7.,305.298925943689,0.0327551936971879));
#11953=CARTESIAN_POINT('Ctrl Pts',(-7.00877672769909,305.436425943689,-1.84288915332067));
#11954=CARTESIAN_POINT('Ctrl Pts',(-6.07855542333967,305.573925943689,-3.47163317015236));
#11955=CARTESIAN_POINT('Ctrl Pts',(-5.14833411898024,305.711425943689,-5.10037718698404));
#11956=CARTESIAN_POINT('Ctrl Pts',(-3.52836682984765,305.848925943689,-6.04580022964248));
#11957=CARTESIAN_POINT('Ctrl Pts',(-1.90839954071505,305.986425943689,-6.99122327230092));
#11958=CARTESIAN_POINT('Ctrl Pts',(-0.0327551936971884,306.123925943689,
-7.));
#11959=CARTESIAN_POINT('Ctrl Pts',(1.84288915332067,306.261425943689,-7.00877672769909));
#11960=CARTESIAN_POINT('Ctrl Pts',(3.47163317015236,306.398925943689,-6.07855542333967));
#11961=CARTESIAN_POINT('Ctrl Pts',(5.10037718698404,306.536425943689,-5.14833411898024));
#11962=CARTESIAN_POINT('Ctrl Pts',(6.04580022964248,306.673925943689,-3.52836682984765));
#11963=CARTESIAN_POINT('Ctrl Pts',(6.99122327230092,306.811425943689,-1.90839954071505));
#11964=CARTESIAN_POINT('Ctrl Pts',(7.,306.948925943689,-0.0327551936971888));
#11965=CARTESIAN_POINT('Ctrl Pts',(7.00877672769909,307.086425943689,1.84288915332067));
#11966=CARTESIAN_POINT('Ctrl Pts',(6.07855542333967,307.223925943689,3.47163317015236));
#11967=CARTESIAN_POINT('Ctrl Pts',(5.14833411898025,307.361425943689,5.10037718698404));
#11968=CARTESIAN_POINT('Ctrl Pts',(3.52836682984765,307.498925943689,6.04580022964248));
#11969=CARTESIAN_POINT('Ctrl Pts',(1.90839954071505,307.636425943689,6.99122327230091));
#11970=CARTESIAN_POINT('Ctrl Pts',(0.0327551936971892,307.773925943689,
7.));
#11971=CARTESIAN_POINT('Ctrl Pts',(-1.84288915332067,307.911425943689,7.00877672769909));
#11972=CARTESIAN_POINT('Ctrl Pts',(-3.47163317015235,308.048925943689,6.07855542333967));
#11973=CARTESIAN_POINT('Ctrl Pts',(-5.10037718698404,308.186425943689,5.14833411898025));
#11974=CARTESIAN_POINT('Ctrl Pts',(-6.04580022964248,308.323925943689,3.52836682984765));
#11975=CARTESIAN_POINT('Ctrl Pts',(-6.99122327230091,308.461425943689,1.90839954071505));
#11976=CARTESIAN_POINT('Ctrl Pts',(-7.,308.598925943689,0.0327551936971879));
#11977=CARTESIAN_POINT('Ctrl Pts',(-7.00877672769909,308.736425943689,-1.84288915332067));
#11978=CARTESIAN_POINT('Ctrl Pts',(-6.07855542333967,308.873925943689,-3.47163317015236));
#11979=CARTESIAN_POINT('Ctrl Pts',(-5.14833411898024,309.011425943689,-5.10037718698404));
#11980=CARTESIAN_POINT('Ctrl Pts',(-3.52836682984765,309.148925943689,-6.04580022964248));
#11981=CARTESIAN_POINT('Ctrl Pts',(-1.90839954071505,309.286425943689,-6.99122327230092));
#11982=CARTESIAN_POINT('Ctrl Pts',(-0.0327551936971884,309.423925943689,
-7.));
#11983=CARTESIAN_POINT('Ctrl Pts',(1.84288915332067,309.561425943689,-7.00877672769909));
#11984=CARTESIAN_POINT('Ctrl Pts',(3.47163317015236,309.698925943689,-6.07855542333967));
#11985=CARTESIAN_POINT('Ctrl Pts',(5.10037718698404,309.836425943689,-5.14833411898024));
#11986=CARTESIAN_POINT('Ctrl Pts',(6.04580022964248,309.973925943689,-3.52836682984765));
#11987=CARTESIAN_POINT('Ctrl Pts',(6.99122327230092,310.111425943689,-1.90839954071505));
#11988=CARTESIAN_POINT('Ctrl Pts',(7.,310.248925943689,-0.0327551936971888));
#11989=CARTESIAN_POINT('Ctrl Pts',(7.00877672769909,310.386425943689,1.84288915332067));
#11990=CARTESIAN_POINT('Ctrl Pts',(6.07855542333967,310.523925943689,3.47163317015236));
#11991=CARTESIAN_POINT('Ctrl Pts',(5.14833411898025,310.661425943689,5.10037718698404));
#11992=CARTESIAN_POINT('Ctrl Pts',(3.52836682984765,310.798925943689,6.04580022964248));
#11993=CARTESIAN_POINT('Ctrl Pts',(1.90839954071505,310.936425943689,6.99122327230091));
#11994=CARTESIAN_POINT('Ctrl Pts',(0.0327551936971892,311.073925943689,
7.));
#11995=CARTESIAN_POINT('Ctrl Pts',(-1.84288915332067,311.211425943689,7.00877672769909));
#11996=CARTESIAN_POINT('Ctrl Pts',(-3.47163317015235,311.348925943689,6.07855542333967));
#11997=CARTESIAN_POINT('Ctrl Pts',(-5.10037718698404,311.486425943689,5.14833411898025));
#11998=CARTESIAN_POINT('Ctrl Pts',(-6.04580022964248,311.623925943689,3.52836682984765));
#11999=CARTESIAN_POINT('Ctrl Pts',(-6.99122327230091,311.761425943689,1.90839954071505));
#12000=CARTESIAN_POINT('Ctrl Pts',(-7.,311.898925943689,0.0327551936971879));
#12001=CARTESIAN_POINT('Ctrl Pts',(-7.00877672769909,312.036425943689,-1.84288915332067));
#12002=CARTESIAN_POINT('Ctrl Pts',(-6.07855542333967,312.173925943689,-3.47163317015236));
#12003=CARTESIAN_POINT('Ctrl Pts',(-5.14833411898024,312.311425943689,-5.10037718698404));
#12004=CARTESIAN_POINT('Ctrl Pts',(-3.52836682984765,312.448925943689,-6.04580022964248));
#12005=CARTESIAN_POINT('Ctrl Pts',(-1.90839954071505,312.586425943689,-6.99122327230092));
#12006=CARTESIAN_POINT('Ctrl Pts',(-0.0327551936971884,312.723925943689,
-7.));
#12007=CARTESIAN_POINT('Ctrl Pts',(1.84288915332067,312.861425943689,-7.00877672769909));
#12008=CARTESIAN_POINT('Ctrl Pts',(3.47163317015236,312.998925943689,-6.07855542333967));
#12009=CARTESIAN_POINT('Ctrl Pts',(5.10037718698404,313.136425943689,-5.14833411898024));
#12010=CARTESIAN_POINT('Ctrl Pts',(6.04580022964248,313.273925943689,-3.52836682984765));
#12011=CARTESIAN_POINT('Ctrl Pts',(6.99122327230092,313.411425943689,-1.90839954071505));
#12012=CARTESIAN_POINT('Ctrl Pts',(7.,313.548925943689,-0.0327551936971888));
#12013=CARTESIAN_POINT('Ctrl Pts',(7.00877672769909,313.686425943689,1.84288915332067));
#12014=CARTESIAN_POINT('Ctrl Pts',(6.07855542333967,313.823925943689,3.47163317015236));
#12015=CARTESIAN_POINT('Ctrl Pts',(5.14833411898025,313.961425943689,5.10037718698404));
#12016=CARTESIAN_POINT('Ctrl Pts',(3.52836682984765,314.098925943689,6.04580022964248));
#12017=CARTESIAN_POINT('Ctrl Pts',(1.90839954071505,314.236425943689,6.99122327230091));
#12018=CARTESIAN_POINT('Ctrl Pts',(0.0327551936971892,314.373925943689,
7.));
#12019=CARTESIAN_POINT('Ctrl Pts',(-1.84288915332067,314.511425943689,7.00877672769909));
#12020=CARTESIAN_POINT('Ctrl Pts',(-3.47163317015235,314.648925943689,6.07855542333967));
#12021=CARTESIAN_POINT('Ctrl Pts',(-5.10037718698404,314.786425943689,5.14833411898025));
#12022=CARTESIAN_POINT('Ctrl Pts',(-6.04580022964248,314.923925943689,3.52836682984765));
#12023=CARTESIAN_POINT('Ctrl Pts',(-6.99122327230091,315.061425943689,1.90839954071505));
#12024=CARTESIAN_POINT('Ctrl Pts',(-7.,315.198925943689,0.0327551936971879));
#12025=CARTESIAN_POINT('Ctrl Pts',(-7.00877672769909,315.336425943689,-1.84288915332067));
#12026=CARTESIAN_POINT('Ctrl Pts',(-6.07855542333967,315.473925943689,-3.47163317015236));
#12027=CARTESIAN_POINT('Ctrl Pts',(-5.14833411898024,315.611425943689,-5.10037718698404));
#12028=CARTESIAN_POINT('Ctrl Pts',(-3.52836682984765,315.748925943689,-6.04580022964248));
#12029=CARTESIAN_POINT('Ctrl Pts',(-1.90839954071505,315.886425943689,-6.99122327230092));
#12030=CARTESIAN_POINT('Ctrl Pts',(-0.0327551936971884,316.023925943689,
-7.));
#12031=CARTESIAN_POINT('Ctrl Pts',(1.84288915332067,316.161425943689,-7.00877672769909));
#12032=CARTESIAN_POINT('Ctrl Pts',(3.47163317015236,316.298925943689,-6.07855542333967));
#12033=CARTESIAN_POINT('Ctrl Pts',(5.10037718698404,316.436425943689,-5.14833411898024));
#12034=CARTESIAN_POINT('Ctrl Pts',(6.04580022964248,316.573925943689,-3.52836682984765));
#12035=CARTESIAN_POINT('Ctrl Pts',(6.99122327230092,316.711425943689,-1.90839954071505));
#12036=CARTESIAN_POINT('Ctrl Pts',(7.,316.848925943689,-0.0327551936971888));
#12037=CARTESIAN_POINT('Ctrl Pts',(7.00877672769909,316.986425943689,1.84288915332067));
#12038=CARTESIAN_POINT('Ctrl Pts',(6.07855542333967,317.123925943689,3.47163317015236));
#12039=CARTESIAN_POINT('Ctrl Pts',(5.14833411898025,317.261425943689,5.10037718698404));
#12040=CARTESIAN_POINT('Ctrl Pts',(3.52836682984765,317.398925943689,6.04580022964248));
#12041=CARTESIAN_POINT('Ctrl Pts',(1.90839954071505,317.536425943689,6.99122327230091));
#12042=CARTESIAN_POINT('Ctrl Pts',(0.0327551936971892,317.673925943689,
7.));
#12043=CARTESIAN_POINT('Ctrl Pts',(-1.84288915332067,317.811425943689,7.00877672769909));
#12044=CARTESIAN_POINT('Ctrl Pts',(-3.47163317015235,317.948925943689,6.07855542333967));
#12045=CARTESIAN_POINT('Ctrl Pts',(-5.10037718698404,318.086425943689,5.14833411898025));
#12046=CARTESIAN_POINT('Ctrl Pts',(-6.04580022964248,318.223925943689,3.52836682984765));
#12047=CARTESIAN_POINT('Ctrl Pts',(-6.99122327230091,318.361425943689,1.90839954071505));
#12048=CARTESIAN_POINT('Ctrl Pts',(-7.,318.498925943689,0.0327551936971879));
#12049=CARTESIAN_POINT('Ctrl Pts',(-7.,284.501074056311,-0.0327551936970413));
#12050=CARTESIAN_POINT('Ctrl Pts',(-6.99122327230096,284.638574056311,-1.9083995407149));
#12051=CARTESIAN_POINT('Ctrl Pts',(-6.04580022964255,284.776074056311,-3.52836682984752));
#12052=CARTESIAN_POINT('Ctrl Pts',(-5.10037718698415,284.913574056311,-5.14833411898014));
#12053=CARTESIAN_POINT('Ctrl Pts',(-3.47163317015249,285.051074056311,-6.07855542333959));
#12054=CARTESIAN_POINT('Ctrl Pts',(-1.84288915332082,285.188574056311,-7.00877672769905));
#12055=CARTESIAN_POINT('Ctrl Pts',(0.0327551936970409,285.326074056311,
-7.));
#12056=CARTESIAN_POINT('Ctrl Pts',(1.9083995407149,285.463574056311,-6.99122327230096));
#12057=CARTESIAN_POINT('Ctrl Pts',(3.52836682984752,285.601074056311,-6.04580022964255));
#12058=CARTESIAN_POINT('Ctrl Pts',(5.14833411898014,285.738574056311,-5.10037718698415));
#12059=CARTESIAN_POINT('Ctrl Pts',(6.07855542333959,285.876074056311,-3.47163317015249));
#12060=CARTESIAN_POINT('Ctrl Pts',(7.00877672769905,286.013574056311,-1.84288915332082));
#12061=CARTESIAN_POINT('Ctrl Pts',(7.,286.151074056311,0.0327551936970405));
#12062=CARTESIAN_POINT('Ctrl Pts',(6.99122327230096,286.288574056311,1.9083995407149));
#12063=CARTESIAN_POINT('Ctrl Pts',(6.04580022964255,286.426074056311,3.52836682984752));
#12064=CARTESIAN_POINT('Ctrl Pts',(5.10037718698415,286.563574056311,5.14833411898013));
#12065=CARTESIAN_POINT('Ctrl Pts',(3.47163317015249,286.701074056311,6.07855542333959));
#12066=CARTESIAN_POINT('Ctrl Pts',(1.84288915332082,286.838574056311,7.00877672769905));
#12067=CARTESIAN_POINT('Ctrl Pts',(-0.03275519369704,286.976074056311,7.));
#12068=CARTESIAN_POINT('Ctrl Pts',(-1.9083995407149,287.113574056311,6.99122327230096));
#12069=CARTESIAN_POINT('Ctrl Pts',(-3.52836682984752,287.251074056311,6.04580022964255));
#12070=CARTESIAN_POINT('Ctrl Pts',(-5.14833411898014,287.388574056311,5.10037718698415));
#12071=CARTESIAN_POINT('Ctrl Pts',(-6.07855542333959,287.526074056311,3.47163317015249));
#12072=CARTESIAN_POINT('Ctrl Pts',(-7.00877672769905,287.663574056311,1.84288915332082));
#12073=CARTESIAN_POINT('Ctrl Pts',(-7.,287.801074056311,-0.0327551936970413));
#12074=CARTESIAN_POINT('Ctrl Pts',(-6.99122327230096,287.938574056311,-1.9083995407149));
#12075=CARTESIAN_POINT('Ctrl Pts',(-6.04580022964255,288.076074056311,-3.52836682984752));
#12076=CARTESIAN_POINT('Ctrl Pts',(-5.10037718698415,288.213574056311,-5.14833411898014));
#12077=CARTESIAN_POINT('Ctrl Pts',(-3.47163317015249,288.351074056311,-6.07855542333959));
#12078=CARTESIAN_POINT('Ctrl Pts',(-1.84288915332082,288.488574056311,-7.00877672769905));
#12079=CARTESIAN_POINT('Ctrl Pts',(0.0327551936970409,288.626074056311,
-7.));
#12080=CARTESIAN_POINT('Ctrl Pts',(1.9083995407149,288.763574056311,-6.99122327230096));
#12081=CARTESIAN_POINT('Ctrl Pts',(3.52836682984752,288.901074056311,-6.04580022964255));
#12082=CARTESIAN_POINT('Ctrl Pts',(5.14833411898014,289.038574056311,-5.10037718698415));
#12083=CARTESIAN_POINT('Ctrl Pts',(6.07855542333959,289.176074056311,-3.47163317015249));
#12084=CARTESIAN_POINT('Ctrl Pts',(7.00877672769905,289.313574056311,-1.84288915332082));
#12085=CARTESIAN_POINT('Ctrl Pts',(7.,289.451074056311,0.0327551936970405));
#12086=CARTESIAN_POINT('Ctrl Pts',(6.99122327230096,289.588574056311,1.9083995407149));
#12087=CARTESIAN_POINT('Ctrl Pts',(6.04580022964255,289.726074056311,3.52836682984752));
#12088=CARTESIAN_POINT('Ctrl Pts',(5.10037718698415,289.863574056311,5.14833411898013));
#12089=CARTESIAN_POINT('Ctrl Pts',(3.47163317015249,290.001074056311,6.07855542333959));
#12090=CARTESIAN_POINT('Ctrl Pts',(1.84288915332082,290.138574056311,7.00877672769905));
#12091=CARTESIAN_POINT('Ctrl Pts',(-0.03275519369704,290.276074056311,7.));
#12092=CARTESIAN_POINT('Ctrl Pts',(-1.9083995407149,290.413574056311,6.99122327230096));
#12093=CARTESIAN_POINT('Ctrl Pts',(-3.52836682984752,290.551074056311,6.04580022964255));
#12094=CARTESIAN_POINT('Ctrl Pts',(-5.14833411898014,290.688574056311,5.10037718698415));
#12095=CARTESIAN_POINT('Ctrl Pts',(-6.07855542333959,290.826074056311,3.47163317015249));
#12096=CARTESIAN_POINT('Ctrl Pts',(-7.00877672769905,290.963574056311,1.84288915332082));
#12097=CARTESIAN_POINT('Ctrl Pts',(-7.,291.101074056311,-0.0327551936970413));
#12098=CARTESIAN_POINT('Ctrl Pts',(-6.99122327230096,291.238574056311,-1.9083995407149));
#12099=CARTESIAN_POINT('Ctrl Pts',(-6.04580022964255,291.376074056311,-3.52836682984752));
#12100=CARTESIAN_POINT('Ctrl Pts',(-5.10037718698415,291.513574056311,-5.14833411898014));
#12101=CARTESIAN_POINT('Ctrl Pts',(-3.47163317015249,291.651074056311,-6.07855542333959));
#12102=CARTESIAN_POINT('Ctrl Pts',(-1.84288915332082,291.788574056311,-7.00877672769905));
#12103=CARTESIAN_POINT('Ctrl Pts',(0.0327551936970409,291.926074056311,
-7.));
#12104=CARTESIAN_POINT('Ctrl Pts',(1.9083995407149,292.063574056311,-6.99122327230096));
#12105=CARTESIAN_POINT('Ctrl Pts',(3.52836682984752,292.201074056311,-6.04580022964255));
#12106=CARTESIAN_POINT('Ctrl Pts',(5.14833411898014,292.338574056311,-5.10037718698415));
#12107=CARTESIAN_POINT('Ctrl Pts',(6.07855542333959,292.476074056311,-3.47163317015249));
#12108=CARTESIAN_POINT('Ctrl Pts',(7.00877672769905,292.613574056311,-1.84288915332082));
#12109=CARTESIAN_POINT('Ctrl Pts',(7.,292.751074056311,0.0327551936970405));
#12110=CARTESIAN_POINT('Ctrl Pts',(6.99122327230096,292.888574056311,1.9083995407149));
#12111=CARTESIAN_POINT('Ctrl Pts',(6.04580022964255,293.026074056311,3.52836682984752));
#12112=CARTESIAN_POINT('Ctrl Pts',(5.10037718698415,293.163574056311,5.14833411898013));
#12113=CARTESIAN_POINT('Ctrl Pts',(3.47163317015249,293.301074056311,6.07855542333959));
#12114=CARTESIAN_POINT('Ctrl Pts',(1.84288915332082,293.438574056311,7.00877672769905));
#12115=CARTESIAN_POINT('Ctrl Pts',(-0.03275519369704,293.576074056311,7.));
#12116=CARTESIAN_POINT('Ctrl Pts',(-1.9083995407149,293.713574056311,6.99122327230096));
#12117=CARTESIAN_POINT('Ctrl Pts',(-3.52836682984752,293.851074056311,6.04580022964255));
#12118=CARTESIAN_POINT('Ctrl Pts',(-5.14833411898014,293.988574056311,5.10037718698415));
#12119=CARTESIAN_POINT('Ctrl Pts',(-6.07855542333959,294.126074056311,3.47163317015249));
#12120=CARTESIAN_POINT('Ctrl Pts',(-7.00877672769905,294.263574056311,1.84288915332082));
#12121=CARTESIAN_POINT('Ctrl Pts',(-7.,294.401074056311,-0.0327551936970413));
#12122=CARTESIAN_POINT('Ctrl Pts',(-6.99122327230096,294.538574056311,-1.9083995407149));
#12123=CARTESIAN_POINT('Ctrl Pts',(-6.04580022964255,294.676074056311,-3.52836682984752));
#12124=CARTESIAN_POINT('Ctrl Pts',(-5.10037718698415,294.813574056311,-5.14833411898014));
#12125=CARTESIAN_POINT('Ctrl Pts',(-3.47163317015249,294.951074056311,-6.07855542333959));
#12126=CARTESIAN_POINT('Ctrl Pts',(-1.84288915332082,295.088574056311,-7.00877672769905));
#12127=CARTESIAN_POINT('Ctrl Pts',(0.0327551936970409,295.226074056311,
-7.));
#12128=CARTESIAN_POINT('Ctrl Pts',(1.9083995407149,295.363574056311,-6.99122327230096));
#12129=CARTESIAN_POINT('Ctrl Pts',(3.52836682984752,295.501074056311,-6.04580022964255));
#12130=CARTESIAN_POINT('Ctrl Pts',(5.14833411898014,295.638574056311,-5.10037718698415));
#12131=CARTESIAN_POINT('Ctrl Pts',(6.07855542333959,295.776074056311,-3.47163317015249));
#12132=CARTESIAN_POINT('Ctrl Pts',(7.00877672769905,295.913574056311,-1.84288915332082));
#12133=CARTESIAN_POINT('Ctrl Pts',(7.,296.051074056311,0.0327551936970405));
#12134=CARTESIAN_POINT('Ctrl Pts',(6.99122327230096,296.188574056311,1.9083995407149));
#12135=CARTESIAN_POINT('Ctrl Pts',(6.04580022964255,296.326074056311,3.52836682984752));
#12136=CARTESIAN_POINT('Ctrl Pts',(5.10037718698415,296.463574056311,5.14833411898013));
#12137=CARTESIAN_POINT('Ctrl Pts',(3.47163317015249,296.601074056311,6.07855542333959));
#12138=CARTESIAN_POINT('Ctrl Pts',(1.84288915332082,296.738574056311,7.00877672769905));
#12139=CARTESIAN_POINT('Ctrl Pts',(-0.03275519369704,296.876074056311,7.));
#12140=CARTESIAN_POINT('Ctrl Pts',(-1.9083995407149,297.013574056311,6.99122327230096));
#12141=CARTESIAN_POINT('Ctrl Pts',(-3.52836682984752,297.151074056311,6.04580022964255));
#12142=CARTESIAN_POINT('Ctrl Pts',(-5.14833411898014,297.288574056311,5.10037718698415));
#12143=CARTESIAN_POINT('Ctrl Pts',(-6.07855542333959,297.426074056311,3.47163317015249));
#12144=CARTESIAN_POINT('Ctrl Pts',(-7.00877672769905,297.563574056311,1.84288915332082));
#12145=CARTESIAN_POINT('Ctrl Pts',(-7.,297.701074056311,-0.0327551936970413));
#12146=CARTESIAN_POINT('Ctrl Pts',(-6.99122327230096,297.838574056311,-1.9083995407149));
#12147=CARTESIAN_POINT('Ctrl Pts',(-6.04580022964255,297.976074056311,-3.52836682984752));
#12148=CARTESIAN_POINT('Ctrl Pts',(-5.10037718698415,298.113574056311,-5.14833411898014));
#12149=CARTESIAN_POINT('Ctrl Pts',(-3.47163317015249,298.251074056311,-6.07855542333959));
#12150=CARTESIAN_POINT('Ctrl Pts',(-1.84288915332082,298.388574056311,-7.00877672769905));
#12151=CARTESIAN_POINT('Ctrl Pts',(0.0327551936970409,298.526074056311,
-7.));
#12152=CARTESIAN_POINT('Ctrl Pts',(1.9083995407149,298.663574056311,-6.99122327230096));
#12153=CARTESIAN_POINT('Ctrl Pts',(3.52836682984752,298.801074056311,-6.04580022964255));
#12154=CARTESIAN_POINT('Ctrl Pts',(5.14833411898014,298.938574056311,-5.10037718698415));
#12155=CARTESIAN_POINT('Ctrl Pts',(6.07855542333959,299.076074056311,-3.47163317015249));
#12156=CARTESIAN_POINT('Ctrl Pts',(7.00877672769905,299.213574056311,-1.84288915332082));
#12157=CARTESIAN_POINT('Ctrl Pts',(7.,299.351074056311,0.0327551936970405));
#12158=CARTESIAN_POINT('Ctrl Pts',(6.99122327230096,299.488574056311,1.9083995407149));
#12159=CARTESIAN_POINT('Ctrl Pts',(6.04580022964255,299.626074056311,3.52836682984752));
#12160=CARTESIAN_POINT('Ctrl Pts',(5.10037718698415,299.763574056311,5.14833411898013));
#12161=CARTESIAN_POINT('Ctrl Pts',(3.47163317015249,299.901074056311,6.07855542333959));
#12162=CARTESIAN_POINT('Ctrl Pts',(1.84288915332082,300.038574056311,7.00877672769905));
#12163=CARTESIAN_POINT('Ctrl Pts',(-0.03275519369704,300.176074056311,7.));
#12164=CARTESIAN_POINT('Ctrl Pts',(-1.9083995407149,300.313574056311,6.99122327230096));
#12165=CARTESIAN_POINT('Ctrl Pts',(-3.52836682984752,300.451074056311,6.04580022964255));
#12166=CARTESIAN_POINT('Ctrl Pts',(-5.14833411898014,300.588574056311,5.10037718698415));
#12167=CARTESIAN_POINT('Ctrl Pts',(-6.07855542333959,300.726074056311,3.47163317015249));
#12168=CARTESIAN_POINT('Ctrl Pts',(-7.00877672769905,300.863574056311,1.84288915332082));
#12169=CARTESIAN_POINT('Ctrl Pts',(-7.,301.001074056311,-0.0327551936970413));
#12170=CARTESIAN_POINT('Ctrl Pts',(-6.99122327230096,301.138574056311,-1.9083995407149));
#12171=CARTESIAN_POINT('Ctrl Pts',(-6.04580022964255,301.276074056311,-3.52836682984752));
#12172=CARTESIAN_POINT('Ctrl Pts',(-5.10037718698415,301.413574056311,-5.14833411898014));
#12173=CARTESIAN_POINT('Ctrl Pts',(-3.47163317015249,301.551074056311,-6.07855542333959));
#12174=CARTESIAN_POINT('Ctrl Pts',(-1.84288915332082,301.688574056311,-7.00877672769905));
#12175=CARTESIAN_POINT('Ctrl Pts',(0.0327551936970409,301.826074056311,
-7.));
#12176=CARTESIAN_POINT('Ctrl Pts',(1.9083995407149,301.963574056311,-6.99122327230096));
#12177=CARTESIAN_POINT('Ctrl Pts',(3.52836682984752,302.101074056311,-6.04580022964255));
#12178=CARTESIAN_POINT('Ctrl Pts',(5.14833411898014,302.238574056311,-5.10037718698415));
#12179=CARTESIAN_POINT('Ctrl Pts',(6.07855542333959,302.376074056311,-3.47163317015249));
#12180=CARTESIAN_POINT('Ctrl Pts',(7.00877672769905,302.513574056311,-1.84288915332082));
#12181=CARTESIAN_POINT('Ctrl Pts',(7.,302.651074056311,0.0327551936970405));
#12182=CARTESIAN_POINT('Ctrl Pts',(6.99122327230096,302.788574056311,1.9083995407149));
#12183=CARTESIAN_POINT('Ctrl Pts',(6.04580022964255,302.926074056311,3.52836682984752));
#12184=CARTESIAN_POINT('Ctrl Pts',(5.10037718698415,303.063574056311,5.14833411898013));
#12185=CARTESIAN_POINT('Ctrl Pts',(3.47163317015249,303.201074056311,6.07855542333959));
#12186=CARTESIAN_POINT('Ctrl Pts',(1.84288915332082,303.338574056311,7.00877672769905));
#12187=CARTESIAN_POINT('Ctrl Pts',(-0.03275519369704,303.476074056311,7.));
#12188=CARTESIAN_POINT('Ctrl Pts',(-1.9083995407149,303.613574056311,6.99122327230096));
#12189=CARTESIAN_POINT('Ctrl Pts',(-3.52836682984752,303.751074056311,6.04580022964255));
#12190=CARTESIAN_POINT('Ctrl Pts',(-5.14833411898014,303.888574056311,5.10037718698415));
#12191=CARTESIAN_POINT('Ctrl Pts',(-6.07855542333959,304.026074056311,3.47163317015249));
#12192=CARTESIAN_POINT('Ctrl Pts',(-7.00877672769905,304.163574056311,1.84288915332082));
#12193=CARTESIAN_POINT('Ctrl Pts',(-7.,304.301074056311,-0.0327551936970413));
#12194=CARTESIAN_POINT('Ctrl Pts',(-6.99122327230096,304.438574056311,-1.9083995407149));
#12195=CARTESIAN_POINT('Ctrl Pts',(-6.04580022964255,304.576074056311,-3.52836682984752));
#12196=CARTESIAN_POINT('Ctrl Pts',(-5.10037718698415,304.713574056311,-5.14833411898014));
#12197=CARTESIAN_POINT('Ctrl Pts',(-3.47163317015249,304.851074056311,-6.07855542333959));
#12198=CARTESIAN_POINT('Ctrl Pts',(-1.84288915332082,304.988574056311,-7.00877672769905));
#12199=CARTESIAN_POINT('Ctrl Pts',(0.0327551936970409,305.126074056311,
-7.));
#12200=CARTESIAN_POINT('Ctrl Pts',(1.9083995407149,305.263574056311,-6.99122327230096));
#12201=CARTESIAN_POINT('Ctrl Pts',(3.52836682984752,305.401074056311,-6.04580022964255));
#12202=CARTESIAN_POINT('Ctrl Pts',(5.14833411898014,305.538574056311,-5.10037718698415));
#12203=CARTESIAN_POINT('Ctrl Pts',(6.07855542333959,305.676074056311,-3.47163317015249));
#12204=CARTESIAN_POINT('Ctrl Pts',(7.00877672769905,305.813574056311,-1.84288915332082));
#12205=CARTESIAN_POINT('Ctrl Pts',(7.,305.951074056311,0.0327551936970405));
#12206=CARTESIAN_POINT('Ctrl Pts',(6.99122327230096,306.088574056311,1.9083995407149));
#12207=CARTESIAN_POINT('Ctrl Pts',(6.04580022964255,306.226074056311,3.52836682984752));
#12208=CARTESIAN_POINT('Ctrl Pts',(5.10037718698415,306.363574056311,5.14833411898013));
#12209=CARTESIAN_POINT('Ctrl Pts',(3.47163317015249,306.501074056311,6.07855542333959));
#12210=CARTESIAN_POINT('Ctrl Pts',(1.84288915332082,306.638574056311,7.00877672769905));
#12211=CARTESIAN_POINT('Ctrl Pts',(-0.03275519369704,306.776074056311,7.));
#12212=CARTESIAN_POINT('Ctrl Pts',(-1.9083995407149,306.913574056311,6.99122327230096));
#12213=CARTESIAN_POINT('Ctrl Pts',(-3.52836682984752,307.051074056311,6.04580022964255));
#12214=CARTESIAN_POINT('Ctrl Pts',(-5.14833411898014,307.188574056311,5.10037718698415));
#12215=CARTESIAN_POINT('Ctrl Pts',(-6.07855542333959,307.326074056311,3.47163317015249));
#12216=CARTESIAN_POINT('Ctrl Pts',(-7.00877672769905,307.463574056311,1.84288915332082));
#12217=CARTESIAN_POINT('Ctrl Pts',(-7.,307.601074056311,-0.0327551936970413));
#12218=CARTESIAN_POINT('Ctrl Pts',(-6.99122327230096,307.738574056311,-1.9083995407149));
#12219=CARTESIAN_POINT('Ctrl Pts',(-6.04580022964255,307.876074056311,-3.52836682984752));
#12220=CARTESIAN_POINT('Ctrl Pts',(-5.10037718698415,308.013574056311,-5.14833411898014));
#12221=CARTESIAN_POINT('Ctrl Pts',(-3.47163317015249,308.151074056311,-6.07855542333959));
#12222=CARTESIAN_POINT('Ctrl Pts',(-1.84288915332082,308.288574056311,-7.00877672769905));
#12223=CARTESIAN_POINT('Ctrl Pts',(0.0327551936970409,308.426074056311,
-7.));
#12224=CARTESIAN_POINT('Ctrl Pts',(1.9083995407149,308.563574056311,-6.99122327230096));
#12225=CARTESIAN_POINT('Ctrl Pts',(3.52836682984752,308.701074056311,-6.04580022964255));
#12226=CARTESIAN_POINT('Ctrl Pts',(5.14833411898014,308.838574056311,-5.10037718698415));
#12227=CARTESIAN_POINT('Ctrl Pts',(6.07855542333959,308.976074056311,-3.47163317015249));
#12228=CARTESIAN_POINT('Ctrl Pts',(7.00877672769905,309.113574056311,-1.84288915332082));
#12229=CARTESIAN_POINT('Ctrl Pts',(7.,309.251074056311,0.0327551936970405));
#12230=CARTESIAN_POINT('Ctrl Pts',(6.99122327230096,309.388574056311,1.9083995407149));
#12231=CARTESIAN_POINT('Ctrl Pts',(6.04580022964255,309.526074056311,3.52836682984752));
#12232=CARTESIAN_POINT('Ctrl Pts',(5.10037718698415,309.663574056311,5.14833411898013));
#12233=CARTESIAN_POINT('Ctrl Pts',(3.47163317015249,309.801074056311,6.07855542333959));
#12234=CARTESIAN_POINT('Ctrl Pts',(1.84288915332082,309.938574056311,7.00877672769905));
#12235=CARTESIAN_POINT('Ctrl Pts',(-0.03275519369704,310.076074056311,7.));
#12236=CARTESIAN_POINT('Ctrl Pts',(-1.9083995407149,310.213574056311,6.99122327230096));
#12237=CARTESIAN_POINT('Ctrl Pts',(-3.52836682984752,310.351074056311,6.04580022964255));
#12238=CARTESIAN_POINT('Ctrl Pts',(-5.14833411898014,310.488574056311,5.10037718698415));
#12239=CARTESIAN_POINT('Ctrl Pts',(-6.07855542333959,310.626074056311,3.47163317015249));
#12240=CARTESIAN_POINT('Ctrl Pts',(-7.00877672769905,310.763574056311,1.84288915332082));
#12241=CARTESIAN_POINT('Ctrl Pts',(-7.,310.901074056311,-0.0327551936970413));
#12242=CARTESIAN_POINT('Ctrl Pts',(-6.99122327230096,311.038574056311,-1.9083995407149));
#12243=CARTESIAN_POINT('Ctrl Pts',(-6.04580022964255,311.176074056311,-3.52836682984752));
#12244=CARTESIAN_POINT('Ctrl Pts',(-5.10037718698415,311.313574056311,-5.14833411898014));
#12245=CARTESIAN_POINT('Ctrl Pts',(-3.47163317015249,311.451074056311,-6.07855542333959));
#12246=CARTESIAN_POINT('Ctrl Pts',(-1.84288915332082,311.588574056311,-7.00877672769905));
#12247=CARTESIAN_POINT('Ctrl Pts',(0.0327551936970409,311.726074056311,
-7.));
#12248=CARTESIAN_POINT('Ctrl Pts',(1.9083995407149,311.863574056311,-6.99122327230096));
#12249=CARTESIAN_POINT('Ctrl Pts',(3.52836682984752,312.001074056311,-6.04580022964255));
#12250=CARTESIAN_POINT('Ctrl Pts',(5.14833411898014,312.138574056311,-5.10037718698415));
#12251=CARTESIAN_POINT('Ctrl Pts',(6.07855542333959,312.276074056311,-3.47163317015249));
#12252=CARTESIAN_POINT('Ctrl Pts',(7.00877672769905,312.413574056311,-1.84288915332082));
#12253=CARTESIAN_POINT('Ctrl Pts',(7.,312.551074056311,0.0327551936970405));
#12254=CARTESIAN_POINT('Ctrl Pts',(6.99122327230096,312.688574056311,1.9083995407149));
#12255=CARTESIAN_POINT('Ctrl Pts',(6.04580022964255,312.826074056311,3.52836682984752));
#12256=CARTESIAN_POINT('Ctrl Pts',(5.10037718698415,312.963574056311,5.14833411898013));
#12257=CARTESIAN_POINT('Ctrl Pts',(3.47163317015249,313.101074056311,6.07855542333959));
#12258=CARTESIAN_POINT('Ctrl Pts',(1.84288915332082,313.238574056311,7.00877672769905));
#12259=CARTESIAN_POINT('Ctrl Pts',(-0.03275519369704,313.376074056311,7.));
#12260=CARTESIAN_POINT('Ctrl Pts',(-1.9083995407149,313.513574056311,6.99122327230096));
#12261=CARTESIAN_POINT('Ctrl Pts',(-3.52836682984752,313.651074056311,6.04580022964255));
#12262=CARTESIAN_POINT('Ctrl Pts',(-5.14833411898014,313.788574056311,5.10037718698415));
#12263=CARTESIAN_POINT('Ctrl Pts',(-6.07855542333959,313.926074056311,3.47163317015249));
#12264=CARTESIAN_POINT('Ctrl Pts',(-7.00877672769905,314.063574056311,1.84288915332082));
#12265=CARTESIAN_POINT('Ctrl Pts',(-7.,314.201074056311,-0.0327551936970413));
#12266=CARTESIAN_POINT('Ctrl Pts',(-6.99122327230096,314.338574056311,-1.9083995407149));
#12267=CARTESIAN_POINT('Ctrl Pts',(-6.04580022964255,314.476074056311,-3.52836682984752));
#12268=CARTESIAN_POINT('Ctrl Pts',(-5.10037718698415,314.613574056311,-5.14833411898014));
#12269=CARTESIAN_POINT('Ctrl Pts',(-3.47163317015249,314.751074056311,-6.07855542333959));
#12270=CARTESIAN_POINT('Ctrl Pts',(-1.84288915332082,314.888574056311,-7.00877672769905));
#12271=CARTESIAN_POINT('Ctrl Pts',(0.0327551936970409,315.026074056311,
-7.));
#12272=CARTESIAN_POINT('Ctrl Pts',(1.9083995407149,315.163574056311,-6.99122327230096));
#12273=CARTESIAN_POINT('Ctrl Pts',(3.52836682984752,315.301074056311,-6.04580022964255));
#12274=CARTESIAN_POINT('Ctrl Pts',(5.14833411898014,315.438574056311,-5.10037718698415));
#12275=CARTESIAN_POINT('Ctrl Pts',(6.07855542333959,315.576074056311,-3.47163317015249));
#12276=CARTESIAN_POINT('Ctrl Pts',(7.00877672769905,315.713574056311,-1.84288915332082));
#12277=CARTESIAN_POINT('Ctrl Pts',(7.,315.851074056311,0.0327551936970405));
#12278=CARTESIAN_POINT('Ctrl Pts',(6.99122327230096,315.988574056311,1.9083995407149));
#12279=CARTESIAN_POINT('Ctrl Pts',(6.04580022964255,316.126074056311,3.52836682984752));
#12280=CARTESIAN_POINT('Ctrl Pts',(5.10037718698415,316.263574056311,5.14833411898013));
#12281=CARTESIAN_POINT('Ctrl Pts',(3.47163317015249,316.401074056311,6.07855542333959));
#12282=CARTESIAN_POINT('Ctrl Pts',(1.84288915332082,316.538574056311,7.00877672769905));
#12283=CARTESIAN_POINT('Ctrl Pts',(-0.03275519369704,316.676074056311,7.));
#12284=CARTESIAN_POINT('Ctrl Pts',(-1.9083995407149,316.813574056311,6.99122327230096));
#12285=CARTESIAN_POINT('Ctrl Pts',(-3.52836682984752,316.951074056311,6.04580022964255));
#12286=CARTESIAN_POINT('Ctrl Pts',(-5.14833411898014,317.088574056311,5.10037718698415));
#12287=CARTESIAN_POINT('Ctrl Pts',(-6.07855542333959,317.226074056311,3.47163317015249));
#12288=CARTESIAN_POINT('Ctrl Pts',(-7.00877672769905,317.363574056311,1.84288915332082));
#12289=CARTESIAN_POINT('Ctrl Pts',(-7.,317.501074056311,-0.0327551936970413));
#12290=CARTESIAN_POINT('Ctrl Pts',(-8.,284.501074056311,-0.0327551936970314));
#12291=CARTESIAN_POINT('Ctrl Pts',(-7.99122327230096,284.638574056311,-2.17634873314601));
#12292=CARTESIAN_POINT('Ctrl Pts',(-6.911825633427,284.776074056311,-4.02836682984751));
#12293=CARTESIAN_POINT('Ctrl Pts',(-5.83242799455303,284.913574056311,-5.88038492654901));
#12294=CARTESIAN_POINT('Ctrl Pts',(-3.97163317015249,285.051074056311,-6.94458082712403));
#12295=CARTESIAN_POINT('Ctrl Pts',(-2.11083834575195,285.188574056311,-8.00877672769905));
#12296=CARTESIAN_POINT('Ctrl Pts',(0.0327551936970309,285.326074056311,
-8.));
#12297=CARTESIAN_POINT('Ctrl Pts',(2.17634873314601,285.463574056311,-7.99122327230096));
#12298=CARTESIAN_POINT('Ctrl Pts',(4.02836682984751,285.601074056311,-6.911825633427));
#12299=CARTESIAN_POINT('Ctrl Pts',(5.88038492654901,285.738574056311,-5.83242799455303));
#12300=CARTESIAN_POINT('Ctrl Pts',(6.94458082712403,285.876074056311,-3.9716331701525));
#12301=CARTESIAN_POINT('Ctrl Pts',(8.00877672769905,286.013574056311,-2.11083834575195));
#12302=CARTESIAN_POINT('Ctrl Pts',(8.,286.151074056311,0.0327551936970304));
#12303=CARTESIAN_POINT('Ctrl Pts',(7.99122327230096,286.288574056311,2.17634873314601));
#12304=CARTESIAN_POINT('Ctrl Pts',(6.911825633427,286.426074056311,4.02836682984751));
#12305=CARTESIAN_POINT('Ctrl Pts',(5.83242799455304,286.563574056311,5.880384926549));
#12306=CARTESIAN_POINT('Ctrl Pts',(3.9716331701525,286.701074056311,6.94458082712403));
#12307=CARTESIAN_POINT('Ctrl Pts',(2.11083834575196,286.838574056311,8.00877672769905));
#12308=CARTESIAN_POINT('Ctrl Pts',(-0.0327551936970299,286.976074056311,
8.));
#12309=CARTESIAN_POINT('Ctrl Pts',(-2.17634873314601,287.113574056311,7.99122327230096));
#12310=CARTESIAN_POINT('Ctrl Pts',(-4.02836682984751,287.251074056311,6.911825633427));
#12311=CARTESIAN_POINT('Ctrl Pts',(-5.88038492654901,287.388574056311,5.83242799455303));
#12312=CARTESIAN_POINT('Ctrl Pts',(-6.94458082712403,287.526074056311,3.9716331701525));
#12313=CARTESIAN_POINT('Ctrl Pts',(-8.00877672769905,287.663574056311,2.11083834575196));
#12314=CARTESIAN_POINT('Ctrl Pts',(-8.,287.801074056311,-0.0327551936970314));
#12315=CARTESIAN_POINT('Ctrl Pts',(-7.99122327230096,287.938574056311,-2.17634873314601));
#12316=CARTESIAN_POINT('Ctrl Pts',(-6.911825633427,288.076074056311,-4.02836682984751));
#12317=CARTESIAN_POINT('Ctrl Pts',(-5.83242799455303,288.213574056311,-5.88038492654901));
#12318=CARTESIAN_POINT('Ctrl Pts',(-3.97163317015249,288.351074056311,-6.94458082712403));
#12319=CARTESIAN_POINT('Ctrl Pts',(-2.11083834575195,288.488574056311,-8.00877672769905));
#12320=CARTESIAN_POINT('Ctrl Pts',(0.0327551936970309,288.626074056311,
-8.));
#12321=CARTESIAN_POINT('Ctrl Pts',(2.17634873314601,288.763574056311,-7.99122327230096));
#12322=CARTESIAN_POINT('Ctrl Pts',(4.02836682984751,288.901074056311,-6.911825633427));
#12323=CARTESIAN_POINT('Ctrl Pts',(5.88038492654901,289.038574056311,-5.83242799455303));
#12324=CARTESIAN_POINT('Ctrl Pts',(6.94458082712403,289.176074056311,-3.9716331701525));
#12325=CARTESIAN_POINT('Ctrl Pts',(8.00877672769905,289.313574056311,-2.11083834575195));
#12326=CARTESIAN_POINT('Ctrl Pts',(8.,289.451074056311,0.0327551936970304));
#12327=CARTESIAN_POINT('Ctrl Pts',(7.99122327230096,289.588574056311,2.17634873314601));
#12328=CARTESIAN_POINT('Ctrl Pts',(6.911825633427,289.726074056311,4.02836682984751));
#12329=CARTESIAN_POINT('Ctrl Pts',(5.83242799455304,289.863574056311,5.880384926549));
#12330=CARTESIAN_POINT('Ctrl Pts',(3.9716331701525,290.001074056311,6.94458082712403));
#12331=CARTESIAN_POINT('Ctrl Pts',(2.11083834575196,290.138574056311,8.00877672769905));
#12332=CARTESIAN_POINT('Ctrl Pts',(-0.0327551936970299,290.276074056311,
8.));
#12333=CARTESIAN_POINT('Ctrl Pts',(-2.17634873314601,290.413574056311,7.99122327230096));
#12334=CARTESIAN_POINT('Ctrl Pts',(-4.02836682984751,290.551074056311,6.911825633427));
#12335=CARTESIAN_POINT('Ctrl Pts',(-5.88038492654901,290.688574056311,5.83242799455303));
#12336=CARTESIAN_POINT('Ctrl Pts',(-6.94458082712403,290.826074056311,3.9716331701525));
#12337=CARTESIAN_POINT('Ctrl Pts',(-8.00877672769905,290.963574056311,2.11083834575196));
#12338=CARTESIAN_POINT('Ctrl Pts',(-8.,291.101074056311,-0.0327551936970314));
#12339=CARTESIAN_POINT('Ctrl Pts',(-7.99122327230096,291.238574056311,-2.17634873314601));
#12340=CARTESIAN_POINT('Ctrl Pts',(-6.911825633427,291.376074056311,-4.02836682984751));
#12341=CARTESIAN_POINT('Ctrl Pts',(-5.83242799455303,291.513574056311,-5.88038492654901));
#12342=CARTESIAN_POINT('Ctrl Pts',(-3.97163317015249,291.651074056311,-6.94458082712403));
#12343=CARTESIAN_POINT('Ctrl Pts',(-2.11083834575195,291.788574056311,-8.00877672769905));
#12344=CARTESIAN_POINT('Ctrl Pts',(0.0327551936970309,291.926074056311,
-8.));
#12345=CARTESIAN_POINT('Ctrl Pts',(2.17634873314601,292.063574056311,-7.99122327230096));
#12346=CARTESIAN_POINT('Ctrl Pts',(4.02836682984751,292.201074056311,-6.911825633427));
#12347=CARTESIAN_POINT('Ctrl Pts',(5.88038492654901,292.338574056311,-5.83242799455303));
#12348=CARTESIAN_POINT('Ctrl Pts',(6.94458082712403,292.476074056311,-3.9716331701525));
#12349=CARTESIAN_POINT('Ctrl Pts',(8.00877672769905,292.613574056311,-2.11083834575195));
#12350=CARTESIAN_POINT('Ctrl Pts',(8.,292.751074056311,0.0327551936970304));
#12351=CARTESIAN_POINT('Ctrl Pts',(7.99122327230096,292.888574056311,2.17634873314601));
#12352=CARTESIAN_POINT('Ctrl Pts',(6.911825633427,293.026074056311,4.02836682984751));
#12353=CARTESIAN_POINT('Ctrl Pts',(5.83242799455304,293.163574056311,5.880384926549));
#12354=CARTESIAN_POINT('Ctrl Pts',(3.9716331701525,293.301074056311,6.94458082712403));
#12355=CARTESIAN_POINT('Ctrl Pts',(2.11083834575196,293.438574056311,8.00877672769905));
#12356=CARTESIAN_POINT('Ctrl Pts',(-0.0327551936970299,293.576074056311,
8.));
#12357=CARTESIAN_POINT('Ctrl Pts',(-2.17634873314601,293.713574056311,7.99122327230096));
#12358=CARTESIAN_POINT('Ctrl Pts',(-4.02836682984751,293.851074056311,6.911825633427));
#12359=CARTESIAN_POINT('Ctrl Pts',(-5.88038492654901,293.988574056311,5.83242799455303));
#12360=CARTESIAN_POINT('Ctrl Pts',(-6.94458082712403,294.126074056311,3.9716331701525));
#12361=CARTESIAN_POINT('Ctrl Pts',(-8.00877672769905,294.263574056311,2.11083834575196));
#12362=CARTESIAN_POINT('Ctrl Pts',(-8.,294.401074056311,-0.0327551936970314));
#12363=CARTESIAN_POINT('Ctrl Pts',(-7.99122327230096,294.538574056311,-2.17634873314601));
#12364=CARTESIAN_POINT('Ctrl Pts',(-6.911825633427,294.676074056311,-4.02836682984751));
#12365=CARTESIAN_POINT('Ctrl Pts',(-5.83242799455303,294.813574056311,-5.88038492654901));
#12366=CARTESIAN_POINT('Ctrl Pts',(-3.97163317015249,294.951074056311,-6.94458082712403));
#12367=CARTESIAN_POINT('Ctrl Pts',(-2.11083834575195,295.088574056311,-8.00877672769905));
#12368=CARTESIAN_POINT('Ctrl Pts',(0.0327551936970309,295.226074056311,
-8.));
#12369=CARTESIAN_POINT('Ctrl Pts',(2.17634873314601,295.363574056311,-7.99122327230096));
#12370=CARTESIAN_POINT('Ctrl Pts',(4.02836682984751,295.501074056311,-6.911825633427));
#12371=CARTESIAN_POINT('Ctrl Pts',(5.88038492654901,295.638574056311,-5.83242799455303));
#12372=CARTESIAN_POINT('Ctrl Pts',(6.94458082712403,295.776074056311,-3.9716331701525));
#12373=CARTESIAN_POINT('Ctrl Pts',(8.00877672769905,295.913574056311,-2.11083834575195));
#12374=CARTESIAN_POINT('Ctrl Pts',(8.,296.051074056311,0.0327551936970304));
#12375=CARTESIAN_POINT('Ctrl Pts',(7.99122327230096,296.188574056311,2.17634873314601));
#12376=CARTESIAN_POINT('Ctrl Pts',(6.911825633427,296.326074056311,4.02836682984751));
#12377=CARTESIAN_POINT('Ctrl Pts',(5.83242799455304,296.463574056311,5.880384926549));
#12378=CARTESIAN_POINT('Ctrl Pts',(3.9716331701525,296.601074056311,6.94458082712403));
#12379=CARTESIAN_POINT('Ctrl Pts',(2.11083834575196,296.738574056311,8.00877672769905));
#12380=CARTESIAN_POINT('Ctrl Pts',(-0.0327551936970299,296.876074056311,
8.));
#12381=CARTESIAN_POINT('Ctrl Pts',(-2.17634873314601,297.013574056311,7.99122327230096));
#12382=CARTESIAN_POINT('Ctrl Pts',(-4.02836682984751,297.151074056311,6.911825633427));
#12383=CARTESIAN_POINT('Ctrl Pts',(-5.88038492654901,297.288574056311,5.83242799455303));
#12384=CARTESIAN_POINT('Ctrl Pts',(-6.94458082712403,297.426074056311,3.9716331701525));
#12385=CARTESIAN_POINT('Ctrl Pts',(-8.00877672769905,297.563574056311,2.11083834575196));
#12386=CARTESIAN_POINT('Ctrl Pts',(-8.,297.701074056311,-0.0327551936970314));
#12387=CARTESIAN_POINT('Ctrl Pts',(-7.99122327230096,297.838574056311,-2.17634873314601));
#12388=CARTESIAN_POINT('Ctrl Pts',(-6.911825633427,297.976074056311,-4.02836682984751));
#12389=CARTESIAN_POINT('Ctrl Pts',(-5.83242799455303,298.113574056311,-5.88038492654901));
#12390=CARTESIAN_POINT('Ctrl Pts',(-3.97163317015249,298.251074056311,-6.94458082712403));
#12391=CARTESIAN_POINT('Ctrl Pts',(-2.11083834575195,298.388574056311,-8.00877672769905));
#12392=CARTESIAN_POINT('Ctrl Pts',(0.0327551936970309,298.526074056311,
-8.));
#12393=CARTESIAN_POINT('Ctrl Pts',(2.17634873314601,298.663574056311,-7.99122327230096));
#12394=CARTESIAN_POINT('Ctrl Pts',(4.02836682984751,298.801074056311,-6.911825633427));
#12395=CARTESIAN_POINT('Ctrl Pts',(5.88038492654901,298.938574056311,-5.83242799455303));
#12396=CARTESIAN_POINT('Ctrl Pts',(6.94458082712403,299.076074056311,-3.9716331701525));
#12397=CARTESIAN_POINT('Ctrl Pts',(8.00877672769905,299.213574056311,-2.11083834575195));
#12398=CARTESIAN_POINT('Ctrl Pts',(8.,299.351074056311,0.0327551936970304));
#12399=CARTESIAN_POINT('Ctrl Pts',(7.99122327230096,299.488574056311,2.17634873314601));
#12400=CARTESIAN_POINT('Ctrl Pts',(6.911825633427,299.626074056311,4.02836682984751));
#12401=CARTESIAN_POINT('Ctrl Pts',(5.83242799455304,299.763574056311,5.880384926549));
#12402=CARTESIAN_POINT('Ctrl Pts',(3.9716331701525,299.901074056311,6.94458082712403));
#12403=CARTESIAN_POINT('Ctrl Pts',(2.11083834575196,300.038574056311,8.00877672769905));
#12404=CARTESIAN_POINT('Ctrl Pts',(-0.0327551936970299,300.176074056311,
8.));
#12405=CARTESIAN_POINT('Ctrl Pts',(-2.17634873314601,300.313574056311,7.99122327230096));
#12406=CARTESIAN_POINT('Ctrl Pts',(-4.02836682984751,300.451074056311,6.911825633427));
#12407=CARTESIAN_POINT('Ctrl Pts',(-5.88038492654901,300.588574056311,5.83242799455303));
#12408=CARTESIAN_POINT('Ctrl Pts',(-6.94458082712403,300.726074056311,3.9716331701525));
#12409=CARTESIAN_POINT('Ctrl Pts',(-8.00877672769905,300.863574056311,2.11083834575196));
#12410=CARTESIAN_POINT('Ctrl Pts',(-8.,301.001074056311,-0.0327551936970314));
#12411=CARTESIAN_POINT('Ctrl Pts',(-7.99122327230096,301.138574056311,-2.17634873314601));
#12412=CARTESIAN_POINT('Ctrl Pts',(-6.911825633427,301.276074056311,-4.02836682984751));
#12413=CARTESIAN_POINT('Ctrl Pts',(-5.83242799455303,301.413574056311,-5.88038492654901));
#12414=CARTESIAN_POINT('Ctrl Pts',(-3.97163317015249,301.551074056311,-6.94458082712403));
#12415=CARTESIAN_POINT('Ctrl Pts',(-2.11083834575195,301.688574056311,-8.00877672769905));
#12416=CARTESIAN_POINT('Ctrl Pts',(0.0327551936970309,301.826074056311,
-8.));
#12417=CARTESIAN_POINT('Ctrl Pts',(2.17634873314601,301.963574056311,-7.99122327230096));
#12418=CARTESIAN_POINT('Ctrl Pts',(4.02836682984751,302.101074056311,-6.911825633427));
#12419=CARTESIAN_POINT('Ctrl Pts',(5.88038492654901,302.238574056311,-5.83242799455303));
#12420=CARTESIAN_POINT('Ctrl Pts',(6.94458082712403,302.376074056311,-3.9716331701525));
#12421=CARTESIAN_POINT('Ctrl Pts',(8.00877672769905,302.513574056311,-2.11083834575195));
#12422=CARTESIAN_POINT('Ctrl Pts',(8.,302.651074056311,0.0327551936970304));
#12423=CARTESIAN_POINT('Ctrl Pts',(7.99122327230096,302.788574056311,2.17634873314601));
#12424=CARTESIAN_POINT('Ctrl Pts',(6.911825633427,302.926074056311,4.02836682984751));
#12425=CARTESIAN_POINT('Ctrl Pts',(5.83242799455304,303.063574056311,5.880384926549));
#12426=CARTESIAN_POINT('Ctrl Pts',(3.9716331701525,303.201074056311,6.94458082712403));
#12427=CARTESIAN_POINT('Ctrl Pts',(2.11083834575196,303.338574056311,8.00877672769905));
#12428=CARTESIAN_POINT('Ctrl Pts',(-0.0327551936970299,303.476074056311,
8.));
#12429=CARTESIAN_POINT('Ctrl Pts',(-2.17634873314601,303.613574056311,7.99122327230096));
#12430=CARTESIAN_POINT('Ctrl Pts',(-4.02836682984751,303.751074056311,6.911825633427));
#12431=CARTESIAN_POINT('Ctrl Pts',(-5.88038492654901,303.888574056311,5.83242799455303));
#12432=CARTESIAN_POINT('Ctrl Pts',(-6.94458082712403,304.026074056311,3.9716331701525));
#12433=CARTESIAN_POINT('Ctrl Pts',(-8.00877672769905,304.163574056311,2.11083834575196));
#12434=CARTESIAN_POINT('Ctrl Pts',(-8.,304.301074056311,-0.0327551936970314));
#12435=CARTESIAN_POINT('Ctrl Pts',(-7.99122327230096,304.438574056311,-2.17634873314601));
#12436=CARTESIAN_POINT('Ctrl Pts',(-6.911825633427,304.576074056311,-4.02836682984751));
#12437=CARTESIAN_POINT('Ctrl Pts',(-5.83242799455303,304.713574056311,-5.88038492654901));
#12438=CARTESIAN_POINT('Ctrl Pts',(-3.97163317015249,304.851074056311,-6.94458082712403));
#12439=CARTESIAN_POINT('Ctrl Pts',(-2.11083834575195,304.988574056311,-8.00877672769905));
#12440=CARTESIAN_POINT('Ctrl Pts',(0.0327551936970309,305.126074056311,
-8.));
#12441=CARTESIAN_POINT('Ctrl Pts',(2.17634873314601,305.263574056311,-7.99122327230096));
#12442=CARTESIAN_POINT('Ctrl Pts',(4.02836682984751,305.401074056311,-6.911825633427));
#12443=CARTESIAN_POINT('Ctrl Pts',(5.88038492654901,305.538574056311,-5.83242799455303));
#12444=CARTESIAN_POINT('Ctrl Pts',(6.94458082712403,305.676074056311,-3.9716331701525));
#12445=CARTESIAN_POINT('Ctrl Pts',(8.00877672769905,305.813574056311,-2.11083834575195));
#12446=CARTESIAN_POINT('Ctrl Pts',(8.,305.951074056311,0.0327551936970304));
#12447=CARTESIAN_POINT('Ctrl Pts',(7.99122327230096,306.088574056311,2.17634873314601));
#12448=CARTESIAN_POINT('Ctrl Pts',(6.911825633427,306.226074056311,4.02836682984751));
#12449=CARTESIAN_POINT('Ctrl Pts',(5.83242799455304,306.363574056311,5.880384926549));
#12450=CARTESIAN_POINT('Ctrl Pts',(3.9716331701525,306.501074056311,6.94458082712403));
#12451=CARTESIAN_POINT('Ctrl Pts',(2.11083834575196,306.638574056311,8.00877672769905));
#12452=CARTESIAN_POINT('Ctrl Pts',(-0.0327551936970299,306.776074056311,
8.));
#12453=CARTESIAN_POINT('Ctrl Pts',(-2.17634873314601,306.913574056311,7.99122327230096));
#12454=CARTESIAN_POINT('Ctrl Pts',(-4.02836682984751,307.051074056311,6.911825633427));
#12455=CARTESIAN_POINT('Ctrl Pts',(-5.88038492654901,307.188574056311,5.83242799455303));
#12456=CARTESIAN_POINT('Ctrl Pts',(-6.94458082712403,307.326074056311,3.9716331701525));
#12457=CARTESIAN_POINT('Ctrl Pts',(-8.00877672769905,307.463574056311,2.11083834575196));
#12458=CARTESIAN_POINT('Ctrl Pts',(-8.,307.601074056311,-0.0327551936970314));
#12459=CARTESIAN_POINT('Ctrl Pts',(-7.99122327230096,307.738574056311,-2.17634873314601));
#12460=CARTESIAN_POINT('Ctrl Pts',(-6.911825633427,307.876074056311,-4.02836682984751));
#12461=CARTESIAN_POINT('Ctrl Pts',(-5.83242799455303,308.013574056311,-5.88038492654901));
#12462=CARTESIAN_POINT('Ctrl Pts',(-3.97163317015249,308.151074056311,-6.94458082712403));
#12463=CARTESIAN_POINT('Ctrl Pts',(-2.11083834575195,308.288574056311,-8.00877672769905));
#12464=CARTESIAN_POINT('Ctrl Pts',(0.0327551936970309,308.426074056311,
-8.));
#12465=CARTESIAN_POINT('Ctrl Pts',(2.17634873314601,308.563574056311,-7.99122327230096));
#12466=CARTESIAN_POINT('Ctrl Pts',(4.02836682984751,308.701074056311,-6.911825633427));
#12467=CARTESIAN_POINT('Ctrl Pts',(5.88038492654901,308.838574056311,-5.83242799455303));
#12468=CARTESIAN_POINT('Ctrl Pts',(6.94458082712403,308.976074056311,-3.9716331701525));
#12469=CARTESIAN_POINT('Ctrl Pts',(8.00877672769905,309.113574056311,-2.11083834575195));
#12470=CARTESIAN_POINT('Ctrl Pts',(8.,309.251074056311,0.0327551936970304));
#12471=CARTESIAN_POINT('Ctrl Pts',(7.99122327230096,309.388574056311,2.17634873314601));
#12472=CARTESIAN_POINT('Ctrl Pts',(6.911825633427,309.526074056311,4.02836682984751));
#12473=CARTESIAN_POINT('Ctrl Pts',(5.83242799455304,309.663574056311,5.880384926549));
#12474=CARTESIAN_POINT('Ctrl Pts',(3.9716331701525,309.801074056311,6.94458082712403));
#12475=CARTESIAN_POINT('Ctrl Pts',(2.11083834575196,309.938574056311,8.00877672769905));
#12476=CARTESIAN_POINT('Ctrl Pts',(-0.0327551936970299,310.076074056311,
8.));
#12477=CARTESIAN_POINT('Ctrl Pts',(-2.17634873314601,310.213574056311,7.99122327230096));
#12478=CARTESIAN_POINT('Ctrl Pts',(-4.02836682984751,310.351074056311,6.911825633427));
#12479=CARTESIAN_POINT('Ctrl Pts',(-5.88038492654901,310.488574056311,5.83242799455303));
#12480=CARTESIAN_POINT('Ctrl Pts',(-6.94458082712403,310.626074056311,3.9716331701525));
#12481=CARTESIAN_POINT('Ctrl Pts',(-8.00877672769905,310.763574056311,2.11083834575196));
#12482=CARTESIAN_POINT('Ctrl Pts',(-8.,310.901074056311,-0.0327551936970314));
#12483=CARTESIAN_POINT('Ctrl Pts',(-7.99122327230096,311.038574056311,-2.17634873314601));
#12484=CARTESIAN_POINT('Ctrl Pts',(-6.911825633427,311.176074056311,-4.02836682984751));
#12485=CARTESIAN_POINT('Ctrl Pts',(-5.83242799455303,311.313574056311,-5.88038492654901));
#12486=CARTESIAN_POINT('Ctrl Pts',(-3.97163317015249,311.451074056311,-6.94458082712403));
#12487=CARTESIAN_POINT('Ctrl Pts',(-2.11083834575195,311.588574056311,-8.00877672769905));
#12488=CARTESIAN_POINT('Ctrl Pts',(0.0327551936970309,311.726074056311,
-8.));
#12489=CARTESIAN_POINT('Ctrl Pts',(2.17634873314601,311.863574056311,-7.99122327230096));
#12490=CARTESIAN_POINT('Ctrl Pts',(4.02836682984751,312.001074056311,-6.911825633427));
#12491=CARTESIAN_POINT('Ctrl Pts',(5.88038492654901,312.138574056311,-5.83242799455303));
#12492=CARTESIAN_POINT('Ctrl Pts',(6.94458082712403,312.276074056311,-3.9716331701525));
#12493=CARTESIAN_POINT('Ctrl Pts',(8.00877672769905,312.413574056311,-2.11083834575195));
#12494=CARTESIAN_POINT('Ctrl Pts',(8.,312.551074056311,0.0327551936970304));
#12495=CARTESIAN_POINT('Ctrl Pts',(7.99122327230096,312.688574056311,2.17634873314601));
#12496=CARTESIAN_POINT('Ctrl Pts',(6.911825633427,312.826074056311,4.02836682984751));
#12497=CARTESIAN_POINT('Ctrl Pts',(5.83242799455304,312.963574056311,5.880384926549));
#12498=CARTESIAN_POINT('Ctrl Pts',(3.9716331701525,313.101074056311,6.94458082712403));
#12499=CARTESIAN_POINT('Ctrl Pts',(2.11083834575196,313.238574056311,8.00877672769905));
#12500=CARTESIAN_POINT('Ctrl Pts',(-0.0327551936970299,313.376074056311,
8.));
#12501=CARTESIAN_POINT('Ctrl Pts',(-2.17634873314601,313.513574056311,7.99122327230096));
#12502=CARTESIAN_POINT('Ctrl Pts',(-4.02836682984751,313.651074056311,6.911825633427));
#12503=CARTESIAN_POINT('Ctrl Pts',(-5.88038492654901,313.788574056311,5.83242799455303));
#12504=CARTESIAN_POINT('Ctrl Pts',(-6.94458082712403,313.926074056311,3.9716331701525));
#12505=CARTESIAN_POINT('Ctrl Pts',(-8.00877672769905,314.063574056311,2.11083834575196));
#12506=CARTESIAN_POINT('Ctrl Pts',(-8.,314.201074056311,-0.0327551936970314));
#12507=CARTESIAN_POINT('Ctrl Pts',(-7.99122327230096,314.338574056311,-2.17634873314601));
#12508=CARTESIAN_POINT('Ctrl Pts',(-6.911825633427,314.476074056311,-4.02836682984751));
#12509=CARTESIAN_POINT('Ctrl Pts',(-5.83242799455303,314.613574056311,-5.88038492654901));
#12510=CARTESIAN_POINT('Ctrl Pts',(-3.97163317015249,314.751074056311,-6.94458082712403));
#12511=CARTESIAN_POINT('Ctrl Pts',(-2.11083834575195,314.888574056311,-8.00877672769905));
#12512=CARTESIAN_POINT('Ctrl Pts',(0.0327551936970309,315.026074056311,
-8.));
#12513=CARTESIAN_POINT('Ctrl Pts',(2.17634873314601,315.163574056311,-7.99122327230096));
#12514=CARTESIAN_POINT('Ctrl Pts',(4.02836682984751,315.301074056311,-6.911825633427));
#12515=CARTESIAN_POINT('Ctrl Pts',(5.88038492654901,315.438574056311,-5.83242799455303));
#12516=CARTESIAN_POINT('Ctrl Pts',(6.94458082712403,315.576074056311,-3.9716331701525));
#12517=CARTESIAN_POINT('Ctrl Pts',(8.00877672769905,315.713574056311,-2.11083834575195));
#12518=CARTESIAN_POINT('Ctrl Pts',(8.,315.851074056311,0.0327551936970304));
#12519=CARTESIAN_POINT('Ctrl Pts',(7.99122327230096,315.988574056311,2.17634873314601));
#12520=CARTESIAN_POINT('Ctrl Pts',(6.911825633427,316.126074056311,4.02836682984751));
#12521=CARTESIAN_POINT('Ctrl Pts',(5.83242799455304,316.263574056311,5.880384926549));
#12522=CARTESIAN_POINT('Ctrl Pts',(3.9716331701525,316.401074056311,6.94458082712403));
#12523=CARTESIAN_POINT('Ctrl Pts',(2.11083834575196,316.538574056311,8.00877672769905));
#12524=CARTESIAN_POINT('Ctrl Pts',(-0.0327551936970299,316.676074056311,
8.));
#12525=CARTESIAN_POINT('Ctrl Pts',(-2.17634873314601,316.813574056311,7.99122327230096));
#12526=CARTESIAN_POINT('Ctrl Pts',(-4.02836682984751,316.951074056311,6.911825633427));
#12527=CARTESIAN_POINT('Ctrl Pts',(-5.88038492654901,317.088574056311,5.83242799455303));
#12528=CARTESIAN_POINT('Ctrl Pts',(-6.94458082712403,317.226074056311,3.9716331701525));
#12529=CARTESIAN_POINT('Ctrl Pts',(-8.00877672769905,317.363574056311,2.11083834575196));
#12530=CARTESIAN_POINT('Ctrl Pts',(-8.,317.501074056311,-0.0327551936970314));
#12531=CARTESIAN_POINT('Ctrl Pts',(-9.,284.501074056311,-0.0327551936970214));
#12532=CARTESIAN_POINT('Ctrl Pts',(-8.99122327230096,284.638574056311,-2.44429792557713));
#12533=CARTESIAN_POINT('Ctrl Pts',(-7.77785103721144,284.776074056311,-4.5283668298475));
#12534=CARTESIAN_POINT('Ctrl Pts',(-6.56447880212192,284.913574056311,-6.61243573411788));
#12535=CARTESIAN_POINT('Ctrl Pts',(-4.4716331701525,285.051074056311,-7.81060623090846));
#12536=CARTESIAN_POINT('Ctrl Pts',(-2.37878753818309,285.188574056311,-9.00877672769904));
#12537=CARTESIAN_POINT('Ctrl Pts',(0.0327551936970209,285.326074056311,
-9.));
#12538=CARTESIAN_POINT('Ctrl Pts',(2.44429792557713,285.463574056311,-8.99122327230096));
#12539=CARTESIAN_POINT('Ctrl Pts',(4.5283668298475,285.601074056311,-7.77785103721144));
#12540=CARTESIAN_POINT('Ctrl Pts',(6.61243573411788,285.738574056311,-6.56447880212192));
#12541=CARTESIAN_POINT('Ctrl Pts',(7.81060623090846,285.876074056311,-4.4716331701525));
#12542=CARTESIAN_POINT('Ctrl Pts',(9.00877672769904,286.013574056311,-2.37878753818309));
#12543=CARTESIAN_POINT('Ctrl Pts',(9.,286.151074056311,0.0327551936970203));
#12544=CARTESIAN_POINT('Ctrl Pts',(8.99122327230096,286.288574056311,2.44429792557712));
#12545=CARTESIAN_POINT('Ctrl Pts',(7.77785103721144,286.426074056311,4.5283668298475));
#12546=CARTESIAN_POINT('Ctrl Pts',(6.56447880212192,286.563574056311,6.61243573411788));
#12547=CARTESIAN_POINT('Ctrl Pts',(4.47163317015251,286.701074056311,7.81060623090846));
#12548=CARTESIAN_POINT('Ctrl Pts',(2.37878753818309,286.838574056311,9.00877672769904));
#12549=CARTESIAN_POINT('Ctrl Pts',(-0.0327551936970198,286.976074056311,
9.));
#12550=CARTESIAN_POINT('Ctrl Pts',(-2.44429792557712,287.113574056311,8.99122327230096));
#12551=CARTESIAN_POINT('Ctrl Pts',(-4.5283668298475,287.251074056311,7.77785103721144));
#12552=CARTESIAN_POINT('Ctrl Pts',(-6.61243573411788,287.388574056311,6.56447880212192));
#12553=CARTESIAN_POINT('Ctrl Pts',(-7.81060623090846,287.526074056311,4.47163317015251));
#12554=CARTESIAN_POINT('Ctrl Pts',(-9.00877672769904,287.663574056311,2.37878753818309));
#12555=CARTESIAN_POINT('Ctrl Pts',(-9.,287.801074056311,-0.0327551936970214));
#12556=CARTESIAN_POINT('Ctrl Pts',(-8.99122327230096,287.938574056311,-2.44429792557713));
#12557=CARTESIAN_POINT('Ctrl Pts',(-7.77785103721144,288.076074056311,-4.5283668298475));
#12558=CARTESIAN_POINT('Ctrl Pts',(-6.56447880212192,288.213574056311,-6.61243573411788));
#12559=CARTESIAN_POINT('Ctrl Pts',(-4.4716331701525,288.351074056311,-7.81060623090846));
#12560=CARTESIAN_POINT('Ctrl Pts',(-2.37878753818309,288.488574056311,-9.00877672769904));
#12561=CARTESIAN_POINT('Ctrl Pts',(0.0327551936970209,288.626074056311,
-9.));
#12562=CARTESIAN_POINT('Ctrl Pts',(2.44429792557713,288.763574056311,-8.99122327230096));
#12563=CARTESIAN_POINT('Ctrl Pts',(4.5283668298475,288.901074056311,-7.77785103721144));
#12564=CARTESIAN_POINT('Ctrl Pts',(6.61243573411788,289.038574056311,-6.56447880212192));
#12565=CARTESIAN_POINT('Ctrl Pts',(7.81060623090846,289.176074056311,-4.4716331701525));
#12566=CARTESIAN_POINT('Ctrl Pts',(9.00877672769904,289.313574056311,-2.37878753818309));
#12567=CARTESIAN_POINT('Ctrl Pts',(9.,289.451074056311,0.0327551936970203));
#12568=CARTESIAN_POINT('Ctrl Pts',(8.99122327230096,289.588574056311,2.44429792557712));
#12569=CARTESIAN_POINT('Ctrl Pts',(7.77785103721144,289.726074056311,4.5283668298475));
#12570=CARTESIAN_POINT('Ctrl Pts',(6.56447880212192,289.863574056311,6.61243573411788));
#12571=CARTESIAN_POINT('Ctrl Pts',(4.47163317015251,290.001074056311,7.81060623090846));
#12572=CARTESIAN_POINT('Ctrl Pts',(2.37878753818309,290.138574056311,9.00877672769904));
#12573=CARTESIAN_POINT('Ctrl Pts',(-0.0327551936970198,290.276074056311,
9.));
#12574=CARTESIAN_POINT('Ctrl Pts',(-2.44429792557712,290.413574056311,8.99122327230096));
#12575=CARTESIAN_POINT('Ctrl Pts',(-4.5283668298475,290.551074056311,7.77785103721144));
#12576=CARTESIAN_POINT('Ctrl Pts',(-6.61243573411788,290.688574056311,6.56447880212192));
#12577=CARTESIAN_POINT('Ctrl Pts',(-7.81060623090846,290.826074056311,4.47163317015251));
#12578=CARTESIAN_POINT('Ctrl Pts',(-9.00877672769904,290.963574056311,2.37878753818309));
#12579=CARTESIAN_POINT('Ctrl Pts',(-9.,291.101074056311,-0.0327551936970214));
#12580=CARTESIAN_POINT('Ctrl Pts',(-8.99122327230096,291.238574056311,-2.44429792557713));
#12581=CARTESIAN_POINT('Ctrl Pts',(-7.77785103721144,291.376074056311,-4.5283668298475));
#12582=CARTESIAN_POINT('Ctrl Pts',(-6.56447880212192,291.513574056311,-6.61243573411788));
#12583=CARTESIAN_POINT('Ctrl Pts',(-4.4716331701525,291.651074056311,-7.81060623090846));
#12584=CARTESIAN_POINT('Ctrl Pts',(-2.37878753818309,291.788574056311,-9.00877672769904));
#12585=CARTESIAN_POINT('Ctrl Pts',(0.0327551936970209,291.926074056311,
-9.));
#12586=CARTESIAN_POINT('Ctrl Pts',(2.44429792557713,292.063574056311,-8.99122327230096));
#12587=CARTESIAN_POINT('Ctrl Pts',(4.5283668298475,292.201074056311,-7.77785103721144));
#12588=CARTESIAN_POINT('Ctrl Pts',(6.61243573411788,292.338574056311,-6.56447880212192));
#12589=CARTESIAN_POINT('Ctrl Pts',(7.81060623090846,292.476074056311,-4.4716331701525));
#12590=CARTESIAN_POINT('Ctrl Pts',(9.00877672769904,292.613574056311,-2.37878753818309));
#12591=CARTESIAN_POINT('Ctrl Pts',(9.,292.751074056311,0.0327551936970203));
#12592=CARTESIAN_POINT('Ctrl Pts',(8.99122327230096,292.888574056311,2.44429792557712));
#12593=CARTESIAN_POINT('Ctrl Pts',(7.77785103721144,293.026074056311,4.5283668298475));
#12594=CARTESIAN_POINT('Ctrl Pts',(6.56447880212192,293.163574056311,6.61243573411788));
#12595=CARTESIAN_POINT('Ctrl Pts',(4.47163317015251,293.301074056311,7.81060623090846));
#12596=CARTESIAN_POINT('Ctrl Pts',(2.37878753818309,293.438574056311,9.00877672769904));
#12597=CARTESIAN_POINT('Ctrl Pts',(-0.0327551936970198,293.576074056311,
9.));
#12598=CARTESIAN_POINT('Ctrl Pts',(-2.44429792557712,293.713574056311,8.99122327230096));
#12599=CARTESIAN_POINT('Ctrl Pts',(-4.5283668298475,293.851074056311,7.77785103721144));
#12600=CARTESIAN_POINT('Ctrl Pts',(-6.61243573411788,293.988574056311,6.56447880212192));
#12601=CARTESIAN_POINT('Ctrl Pts',(-7.81060623090846,294.126074056311,4.47163317015251));
#12602=CARTESIAN_POINT('Ctrl Pts',(-9.00877672769904,294.263574056311,2.37878753818309));
#12603=CARTESIAN_POINT('Ctrl Pts',(-9.,294.401074056311,-0.0327551936970214));
#12604=CARTESIAN_POINT('Ctrl Pts',(-8.99122327230096,294.538574056311,-2.44429792557713));
#12605=CARTESIAN_POINT('Ctrl Pts',(-7.77785103721144,294.676074056311,-4.5283668298475));
#12606=CARTESIAN_POINT('Ctrl Pts',(-6.56447880212192,294.813574056311,-6.61243573411788));
#12607=CARTESIAN_POINT('Ctrl Pts',(-4.4716331701525,294.951074056311,-7.81060623090846));
#12608=CARTESIAN_POINT('Ctrl Pts',(-2.37878753818309,295.088574056311,-9.00877672769904));
#12609=CARTESIAN_POINT('Ctrl Pts',(0.0327551936970209,295.226074056311,
-9.));
#12610=CARTESIAN_POINT('Ctrl Pts',(2.44429792557713,295.363574056311,-8.99122327230096));
#12611=CARTESIAN_POINT('Ctrl Pts',(4.5283668298475,295.501074056311,-7.77785103721144));
#12612=CARTESIAN_POINT('Ctrl Pts',(6.61243573411788,295.638574056311,-6.56447880212192));
#12613=CARTESIAN_POINT('Ctrl Pts',(7.81060623090846,295.776074056311,-4.4716331701525));
#12614=CARTESIAN_POINT('Ctrl Pts',(9.00877672769904,295.913574056311,-2.37878753818309));
#12615=CARTESIAN_POINT('Ctrl Pts',(9.,296.051074056311,0.0327551936970203));
#12616=CARTESIAN_POINT('Ctrl Pts',(8.99122327230096,296.188574056311,2.44429792557712));
#12617=CARTESIAN_POINT('Ctrl Pts',(7.77785103721144,296.326074056311,4.5283668298475));
#12618=CARTESIAN_POINT('Ctrl Pts',(6.56447880212192,296.463574056311,6.61243573411788));
#12619=CARTESIAN_POINT('Ctrl Pts',(4.47163317015251,296.601074056311,7.81060623090846));
#12620=CARTESIAN_POINT('Ctrl Pts',(2.37878753818309,296.738574056311,9.00877672769904));
#12621=CARTESIAN_POINT('Ctrl Pts',(-0.0327551936970198,296.876074056311,
9.));
#12622=CARTESIAN_POINT('Ctrl Pts',(-2.44429792557712,297.013574056311,8.99122327230096));
#12623=CARTESIAN_POINT('Ctrl Pts',(-4.5283668298475,297.151074056311,7.77785103721144));
#12624=CARTESIAN_POINT('Ctrl Pts',(-6.61243573411788,297.288574056311,6.56447880212192));
#12625=CARTESIAN_POINT('Ctrl Pts',(-7.81060623090846,297.426074056311,4.47163317015251));
#12626=CARTESIAN_POINT('Ctrl Pts',(-9.00877672769904,297.563574056311,2.37878753818309));
#12627=CARTESIAN_POINT('Ctrl Pts',(-9.,297.701074056311,-0.0327551936970214));
#12628=CARTESIAN_POINT('Ctrl Pts',(-8.99122327230096,297.838574056311,-2.44429792557713));
#12629=CARTESIAN_POINT('Ctrl Pts',(-7.77785103721144,297.976074056311,-4.5283668298475));
#12630=CARTESIAN_POINT('Ctrl Pts',(-6.56447880212192,298.113574056311,-6.61243573411788));
#12631=CARTESIAN_POINT('Ctrl Pts',(-4.4716331701525,298.251074056311,-7.81060623090846));
#12632=CARTESIAN_POINT('Ctrl Pts',(-2.37878753818309,298.388574056311,-9.00877672769904));
#12633=CARTESIAN_POINT('Ctrl Pts',(0.0327551936970209,298.526074056311,
-9.));
#12634=CARTESIAN_POINT('Ctrl Pts',(2.44429792557713,298.663574056311,-8.99122327230096));
#12635=CARTESIAN_POINT('Ctrl Pts',(4.5283668298475,298.801074056311,-7.77785103721144));
#12636=CARTESIAN_POINT('Ctrl Pts',(6.61243573411788,298.938574056311,-6.56447880212192));
#12637=CARTESIAN_POINT('Ctrl Pts',(7.81060623090846,299.076074056311,-4.4716331701525));
#12638=CARTESIAN_POINT('Ctrl Pts',(9.00877672769904,299.213574056311,-2.37878753818309));
#12639=CARTESIAN_POINT('Ctrl Pts',(9.,299.351074056311,0.0327551936970203));
#12640=CARTESIAN_POINT('Ctrl Pts',(8.99122327230096,299.488574056311,2.44429792557712));
#12641=CARTESIAN_POINT('Ctrl Pts',(7.77785103721144,299.626074056311,4.5283668298475));
#12642=CARTESIAN_POINT('Ctrl Pts',(6.56447880212192,299.763574056311,6.61243573411788));
#12643=CARTESIAN_POINT('Ctrl Pts',(4.47163317015251,299.901074056311,7.81060623090846));
#12644=CARTESIAN_POINT('Ctrl Pts',(2.37878753818309,300.038574056311,9.00877672769904));
#12645=CARTESIAN_POINT('Ctrl Pts',(-0.0327551936970198,300.176074056311,
9.));
#12646=CARTESIAN_POINT('Ctrl Pts',(-2.44429792557712,300.313574056311,8.99122327230096));
#12647=CARTESIAN_POINT('Ctrl Pts',(-4.5283668298475,300.451074056311,7.77785103721144));
#12648=CARTESIAN_POINT('Ctrl Pts',(-6.61243573411788,300.588574056311,6.56447880212192));
#12649=CARTESIAN_POINT('Ctrl Pts',(-7.81060623090846,300.726074056311,4.47163317015251));
#12650=CARTESIAN_POINT('Ctrl Pts',(-9.00877672769904,300.863574056311,2.37878753818309));
#12651=CARTESIAN_POINT('Ctrl Pts',(-9.,301.001074056311,-0.0327551936970214));
#12652=CARTESIAN_POINT('Ctrl Pts',(-8.99122327230096,301.138574056311,-2.44429792557713));
#12653=CARTESIAN_POINT('Ctrl Pts',(-7.77785103721144,301.276074056311,-4.5283668298475));
#12654=CARTESIAN_POINT('Ctrl Pts',(-6.56447880212192,301.413574056311,-6.61243573411788));
#12655=CARTESIAN_POINT('Ctrl Pts',(-4.4716331701525,301.551074056311,-7.81060623090846));
#12656=CARTESIAN_POINT('Ctrl Pts',(-2.37878753818309,301.688574056311,-9.00877672769904));
#12657=CARTESIAN_POINT('Ctrl Pts',(0.0327551936970209,301.826074056311,
-9.));
#12658=CARTESIAN_POINT('Ctrl Pts',(2.44429792557713,301.963574056311,-8.99122327230096));
#12659=CARTESIAN_POINT('Ctrl Pts',(4.5283668298475,302.101074056311,-7.77785103721144));
#12660=CARTESIAN_POINT('Ctrl Pts',(6.61243573411788,302.238574056311,-6.56447880212192));
#12661=CARTESIAN_POINT('Ctrl Pts',(7.81060623090846,302.376074056311,-4.4716331701525));
#12662=CARTESIAN_POINT('Ctrl Pts',(9.00877672769904,302.513574056311,-2.37878753818309));
#12663=CARTESIAN_POINT('Ctrl Pts',(9.,302.651074056311,0.0327551936970203));
#12664=CARTESIAN_POINT('Ctrl Pts',(8.99122327230096,302.788574056311,2.44429792557712));
#12665=CARTESIAN_POINT('Ctrl Pts',(7.77785103721144,302.926074056311,4.5283668298475));
#12666=CARTESIAN_POINT('Ctrl Pts',(6.56447880212192,303.063574056311,6.61243573411788));
#12667=CARTESIAN_POINT('Ctrl Pts',(4.47163317015251,303.201074056311,7.81060623090846));
#12668=CARTESIAN_POINT('Ctrl Pts',(2.37878753818309,303.338574056311,9.00877672769904));
#12669=CARTESIAN_POINT('Ctrl Pts',(-0.0327551936970198,303.476074056311,
9.));
#12670=CARTESIAN_POINT('Ctrl Pts',(-2.44429792557712,303.613574056311,8.99122327230096));
#12671=CARTESIAN_POINT('Ctrl Pts',(-4.5283668298475,303.751074056311,7.77785103721144));
#12672=CARTESIAN_POINT('Ctrl Pts',(-6.61243573411788,303.888574056311,6.56447880212192));
#12673=CARTESIAN_POINT('Ctrl Pts',(-7.81060623090846,304.026074056311,4.47163317015251));
#12674=CARTESIAN_POINT('Ctrl Pts',(-9.00877672769904,304.163574056311,2.37878753818309));
#12675=CARTESIAN_POINT('Ctrl Pts',(-9.,304.301074056311,-0.0327551936970214));
#12676=CARTESIAN_POINT('Ctrl Pts',(-8.99122327230096,304.438574056311,-2.44429792557713));
#12677=CARTESIAN_POINT('Ctrl Pts',(-7.77785103721144,304.576074056311,-4.5283668298475));
#12678=CARTESIAN_POINT('Ctrl Pts',(-6.56447880212192,304.713574056311,-6.61243573411788));
#12679=CARTESIAN_POINT('Ctrl Pts',(-4.4716331701525,304.851074056311,-7.81060623090846));
#12680=CARTESIAN_POINT('Ctrl Pts',(-2.37878753818309,304.988574056311,-9.00877672769904));
#12681=CARTESIAN_POINT('Ctrl Pts',(0.0327551936970209,305.126074056311,
-9.));
#12682=CARTESIAN_POINT('Ctrl Pts',(2.44429792557713,305.263574056311,-8.99122327230096));
#12683=CARTESIAN_POINT('Ctrl Pts',(4.5283668298475,305.401074056311,-7.77785103721144));
#12684=CARTESIAN_POINT('Ctrl Pts',(6.61243573411788,305.538574056311,-6.56447880212192));
#12685=CARTESIAN_POINT('Ctrl Pts',(7.81060623090846,305.676074056311,-4.4716331701525));
#12686=CARTESIAN_POINT('Ctrl Pts',(9.00877672769904,305.813574056311,-2.37878753818309));
#12687=CARTESIAN_POINT('Ctrl Pts',(9.,305.951074056311,0.0327551936970203));
#12688=CARTESIAN_POINT('Ctrl Pts',(8.99122327230096,306.088574056311,2.44429792557712));
#12689=CARTESIAN_POINT('Ctrl Pts',(7.77785103721144,306.226074056311,4.5283668298475));
#12690=CARTESIAN_POINT('Ctrl Pts',(6.56447880212192,306.363574056311,6.61243573411788));
#12691=CARTESIAN_POINT('Ctrl Pts',(4.47163317015251,306.501074056311,7.81060623090846));
#12692=CARTESIAN_POINT('Ctrl Pts',(2.37878753818309,306.638574056311,9.00877672769904));
#12693=CARTESIAN_POINT('Ctrl Pts',(-0.0327551936970198,306.776074056311,
9.));
#12694=CARTESIAN_POINT('Ctrl Pts',(-2.44429792557712,306.913574056311,8.99122327230096));
#12695=CARTESIAN_POINT('Ctrl Pts',(-4.5283668298475,307.051074056311,7.77785103721144));
#12696=CARTESIAN_POINT('Ctrl Pts',(-6.61243573411788,307.188574056311,6.56447880212192));
#12697=CARTESIAN_POINT('Ctrl Pts',(-7.81060623090846,307.326074056311,4.47163317015251));
#12698=CARTESIAN_POINT('Ctrl Pts',(-9.00877672769904,307.463574056311,2.37878753818309));
#12699=CARTESIAN_POINT('Ctrl Pts',(-9.,307.601074056311,-0.0327551936970214));
#12700=CARTESIAN_POINT('Ctrl Pts',(-8.99122327230096,307.738574056311,-2.44429792557713));
#12701=CARTESIAN_POINT('Ctrl Pts',(-7.77785103721144,307.876074056311,-4.5283668298475));
#12702=CARTESIAN_POINT('Ctrl Pts',(-6.56447880212192,308.013574056311,-6.61243573411788));
#12703=CARTESIAN_POINT('Ctrl Pts',(-4.4716331701525,308.151074056311,-7.81060623090846));
#12704=CARTESIAN_POINT('Ctrl Pts',(-2.37878753818309,308.288574056311,-9.00877672769904));
#12705=CARTESIAN_POINT('Ctrl Pts',(0.0327551936970209,308.426074056311,
-9.));
#12706=CARTESIAN_POINT('Ctrl Pts',(2.44429792557713,308.563574056311,-8.99122327230096));
#12707=CARTESIAN_POINT('Ctrl Pts',(4.5283668298475,308.701074056311,-7.77785103721144));
#12708=CARTESIAN_POINT('Ctrl Pts',(6.61243573411788,308.838574056311,-6.56447880212192));
#12709=CARTESIAN_POINT('Ctrl Pts',(7.81060623090846,308.976074056311,-4.4716331701525));
#12710=CARTESIAN_POINT('Ctrl Pts',(9.00877672769904,309.113574056311,-2.37878753818309));
#12711=CARTESIAN_POINT('Ctrl Pts',(9.,309.251074056311,0.0327551936970203));
#12712=CARTESIAN_POINT('Ctrl Pts',(8.99122327230096,309.388574056311,2.44429792557712));
#12713=CARTESIAN_POINT('Ctrl Pts',(7.77785103721144,309.526074056311,4.5283668298475));
#12714=CARTESIAN_POINT('Ctrl Pts',(6.56447880212192,309.663574056311,6.61243573411788));
#12715=CARTESIAN_POINT('Ctrl Pts',(4.47163317015251,309.801074056311,7.81060623090846));
#12716=CARTESIAN_POINT('Ctrl Pts',(2.37878753818309,309.938574056311,9.00877672769904));
#12717=CARTESIAN_POINT('Ctrl Pts',(-0.0327551936970198,310.076074056311,
9.));
#12718=CARTESIAN_POINT('Ctrl Pts',(-2.44429792557712,310.213574056311,8.99122327230096));
#12719=CARTESIAN_POINT('Ctrl Pts',(-4.5283668298475,310.351074056311,7.77785103721144));
#12720=CARTESIAN_POINT('Ctrl Pts',(-6.61243573411788,310.488574056311,6.56447880212192));
#12721=CARTESIAN_POINT('Ctrl Pts',(-7.81060623090846,310.626074056311,4.47163317015251));
#12722=CARTESIAN_POINT('Ctrl Pts',(-9.00877672769904,310.763574056311,2.37878753818309));
#12723=CARTESIAN_POINT('Ctrl Pts',(-9.,310.901074056311,-0.0327551936970214));
#12724=CARTESIAN_POINT('Ctrl Pts',(-8.99122327230096,311.038574056311,-2.44429792557713));
#12725=CARTESIAN_POINT('Ctrl Pts',(-7.77785103721144,311.176074056311,-4.5283668298475));
#12726=CARTESIAN_POINT('Ctrl Pts',(-6.56447880212192,311.313574056311,-6.61243573411788));
#12727=CARTESIAN_POINT('Ctrl Pts',(-4.4716331701525,311.451074056311,-7.81060623090846));
#12728=CARTESIAN_POINT('Ctrl Pts',(-2.37878753818309,311.588574056311,-9.00877672769904));
#12729=CARTESIAN_POINT('Ctrl Pts',(0.0327551936970209,311.726074056311,
-9.));
#12730=CARTESIAN_POINT('Ctrl Pts',(2.44429792557713,311.863574056311,-8.99122327230096));
#12731=CARTESIAN_POINT('Ctrl Pts',(4.5283668298475,312.001074056311,-7.77785103721144));
#12732=CARTESIAN_POINT('Ctrl Pts',(6.61243573411788,312.138574056311,-6.56447880212192));
#12733=CARTESIAN_POINT('Ctrl Pts',(7.81060623090846,312.276074056311,-4.4716331701525));
#12734=CARTESIAN_POINT('Ctrl Pts',(9.00877672769904,312.413574056311,-2.37878753818309));
#12735=CARTESIAN_POINT('Ctrl Pts',(9.,312.551074056311,0.0327551936970203));
#12736=CARTESIAN_POINT('Ctrl Pts',(8.99122327230096,312.688574056311,2.44429792557712));
#12737=CARTESIAN_POINT('Ctrl Pts',(7.77785103721144,312.826074056311,4.5283668298475));
#12738=CARTESIAN_POINT('Ctrl Pts',(6.56447880212192,312.963574056311,6.61243573411788));
#12739=CARTESIAN_POINT('Ctrl Pts',(4.47163317015251,313.101074056311,7.81060623090846));
#12740=CARTESIAN_POINT('Ctrl Pts',(2.37878753818309,313.238574056311,9.00877672769904));
#12741=CARTESIAN_POINT('Ctrl Pts',(-0.0327551936970198,313.376074056311,
9.));
#12742=CARTESIAN_POINT('Ctrl Pts',(-2.44429792557712,313.513574056311,8.99122327230096));
#12743=CARTESIAN_POINT('Ctrl Pts',(-4.5283668298475,313.651074056311,7.77785103721144));
#12744=CARTESIAN_POINT('Ctrl Pts',(-6.61243573411788,313.788574056311,6.56447880212192));
#12745=CARTESIAN_POINT('Ctrl Pts',(-7.81060623090846,313.926074056311,4.47163317015251));
#12746=CARTESIAN_POINT('Ctrl Pts',(-9.00877672769904,314.063574056311,2.37878753818309));
#12747=CARTESIAN_POINT('Ctrl Pts',(-9.,314.201074056311,-0.0327551936970214));
#12748=CARTESIAN_POINT('Ctrl Pts',(-8.99122327230096,314.338574056311,-2.44429792557713));
#12749=CARTESIAN_POINT('Ctrl Pts',(-7.77785103721144,314.476074056311,-4.5283668298475));
#12750=CARTESIAN_POINT('Ctrl Pts',(-6.56447880212192,314.613574056311,-6.61243573411788));
#12751=CARTESIAN_POINT('Ctrl Pts',(-4.4716331701525,314.751074056311,-7.81060623090846));
#12752=CARTESIAN_POINT('Ctrl Pts',(-2.37878753818309,314.888574056311,-9.00877672769904));
#12753=CARTESIAN_POINT('Ctrl Pts',(0.0327551936970209,315.026074056311,
-9.));
#12754=CARTESIAN_POINT('Ctrl Pts',(2.44429792557713,315.163574056311,-8.99122327230096));
#12755=CARTESIAN_POINT('Ctrl Pts',(4.5283668298475,315.301074056311,-7.77785103721144));
#12756=CARTESIAN_POINT('Ctrl Pts',(6.61243573411788,315.438574056311,-6.56447880212192));
#12757=CARTESIAN_POINT('Ctrl Pts',(7.81060623090846,315.576074056311,-4.4716331701525));
#12758=CARTESIAN_POINT('Ctrl Pts',(9.00877672769904,315.713574056311,-2.37878753818309));
#12759=CARTESIAN_POINT('Ctrl Pts',(9.,315.851074056311,0.0327551936970203));
#12760=CARTESIAN_POINT('Ctrl Pts',(8.99122327230096,315.988574056311,2.44429792557712));
#12761=CARTESIAN_POINT('Ctrl Pts',(7.77785103721144,316.126074056311,4.5283668298475));
#12762=CARTESIAN_POINT('Ctrl Pts',(6.56447880212192,316.263574056311,6.61243573411788));
#12763=CARTESIAN_POINT('Ctrl Pts',(4.47163317015251,316.401074056311,7.81060623090846));
#12764=CARTESIAN_POINT('Ctrl Pts',(2.37878753818309,316.538574056311,9.00877672769904));
#12765=CARTESIAN_POINT('Ctrl Pts',(-0.0327551936970198,316.676074056311,
9.));
#12766=CARTESIAN_POINT('Ctrl Pts',(-2.44429792557712,316.813574056311,8.99122327230096));
#12767=CARTESIAN_POINT('Ctrl Pts',(-4.5283668298475,316.951074056311,7.77785103721144));
#12768=CARTESIAN_POINT('Ctrl Pts',(-6.61243573411788,317.088574056311,6.56447880212192));
#12769=CARTESIAN_POINT('Ctrl Pts',(-7.81060623090846,317.226074056311,4.47163317015251));
#12770=CARTESIAN_POINT('Ctrl Pts',(-9.00877672769904,317.363574056311,2.37878753818309));
#12771=CARTESIAN_POINT('Ctrl Pts',(-9.,317.501074056311,-0.0327551936970214));
#12772=CARTESIAN_POINT('Ctrl Pts',(-9.,285.498925943689,0.0327551936972079));
#12773=CARTESIAN_POINT('Ctrl Pts',(-9.0087767276991,285.636425943689,-2.3787875381829));
#12774=CARTESIAN_POINT('Ctrl Pts',(-7.81060623090856,285.773925943689,-4.47163317015234));
#12775=CARTESIAN_POINT('Ctrl Pts',(-6.61243573411802,285.911425943689,-6.56447880212179));
#12776=CARTESIAN_POINT('Ctrl Pts',(-4.52836682984766,286.048925943689,-7.77785103721135));
#12777=CARTESIAN_POINT('Ctrl Pts',(-2.44429792557731,286.186425943689,-8.99122327230091));
#12778=CARTESIAN_POINT('Ctrl Pts',(-0.0327551936972084,286.323925943689,
-9.));
#12779=CARTESIAN_POINT('Ctrl Pts',(2.3787875381829,286.461425943689,-9.0087767276991));
#12780=CARTESIAN_POINT('Ctrl Pts',(4.47163317015234,286.598925943689,-7.81060623090856));
#12781=CARTESIAN_POINT('Ctrl Pts',(6.56447880212178,286.736425943689,-6.61243573411802));
#12782=CARTESIAN_POINT('Ctrl Pts',(7.77785103721135,286.873925943689,-4.52836682984767));
#12783=CARTESIAN_POINT('Ctrl Pts',(8.99122327230091,287.011425943689,-2.44429792557732));
#12784=CARTESIAN_POINT('Ctrl Pts',(9.,287.148925943689,-0.032755193697209));
#12785=CARTESIAN_POINT('Ctrl Pts',(9.0087767276991,287.286425943689,2.37878753818289));
#12786=CARTESIAN_POINT('Ctrl Pts',(7.81060623090856,287.423925943689,4.47163317015234));
#12787=CARTESIAN_POINT('Ctrl Pts',(6.61243573411802,287.561425943689,6.56447880212178));
#12788=CARTESIAN_POINT('Ctrl Pts',(4.52836682984767,287.698925943689,7.77785103721135));
#12789=CARTESIAN_POINT('Ctrl Pts',(2.44429792557732,287.836425943689,8.99122327230091));
#12790=CARTESIAN_POINT('Ctrl Pts',(0.0327551936972095,287.973925943689,
9.));
#12791=CARTESIAN_POINT('Ctrl Pts',(-2.37878753818289,288.111425943689,9.0087767276991));
#12792=CARTESIAN_POINT('Ctrl Pts',(-4.47163317015233,288.248925943689,7.81060623090856));
#12793=CARTESIAN_POINT('Ctrl Pts',(-6.56447880212178,288.386425943689,6.61243573411802));
#12794=CARTESIAN_POINT('Ctrl Pts',(-7.77785103721135,288.523925943689,4.52836682984767));
#12795=CARTESIAN_POINT('Ctrl Pts',(-8.99122327230091,288.661425943689,2.44429792557732));
#12796=CARTESIAN_POINT('Ctrl Pts',(-9.,288.798925943689,0.0327551936972079));
#12797=CARTESIAN_POINT('Ctrl Pts',(-9.0087767276991,288.936425943689,-2.3787875381829));
#12798=CARTESIAN_POINT('Ctrl Pts',(-7.81060623090856,289.073925943689,-4.47163317015234));
#12799=CARTESIAN_POINT('Ctrl Pts',(-6.61243573411802,289.211425943689,-6.56447880212179));
#12800=CARTESIAN_POINT('Ctrl Pts',(-4.52836682984766,289.348925943689,-7.77785103721135));
#12801=CARTESIAN_POINT('Ctrl Pts',(-2.44429792557731,289.486425943689,-8.99122327230091));
#12802=CARTESIAN_POINT('Ctrl Pts',(-0.0327551936972084,289.623925943689,
-9.));
#12803=CARTESIAN_POINT('Ctrl Pts',(2.3787875381829,289.761425943689,-9.0087767276991));
#12804=CARTESIAN_POINT('Ctrl Pts',(4.47163317015234,289.898925943689,-7.81060623090856));
#12805=CARTESIAN_POINT('Ctrl Pts',(6.56447880212178,290.036425943689,-6.61243573411802));
#12806=CARTESIAN_POINT('Ctrl Pts',(7.77785103721135,290.173925943689,-4.52836682984767));
#12807=CARTESIAN_POINT('Ctrl Pts',(8.99122327230091,290.311425943689,-2.44429792557732));
#12808=CARTESIAN_POINT('Ctrl Pts',(9.,290.448925943689,-0.032755193697209));
#12809=CARTESIAN_POINT('Ctrl Pts',(9.0087767276991,290.586425943689,2.37878753818289));
#12810=CARTESIAN_POINT('Ctrl Pts',(7.81060623090856,290.723925943689,4.47163317015234));
#12811=CARTESIAN_POINT('Ctrl Pts',(6.61243573411802,290.861425943689,6.56447880212178));
#12812=CARTESIAN_POINT('Ctrl Pts',(4.52836682984767,290.998925943689,7.77785103721135));
#12813=CARTESIAN_POINT('Ctrl Pts',(2.44429792557732,291.136425943689,8.99122327230091));
#12814=CARTESIAN_POINT('Ctrl Pts',(0.0327551936972095,291.273925943689,
9.));
#12815=CARTESIAN_POINT('Ctrl Pts',(-2.37878753818289,291.411425943689,9.0087767276991));
#12816=CARTESIAN_POINT('Ctrl Pts',(-4.47163317015233,291.548925943689,7.81060623090856));
#12817=CARTESIAN_POINT('Ctrl Pts',(-6.56447880212178,291.686425943689,6.61243573411802));
#12818=CARTESIAN_POINT('Ctrl Pts',(-7.77785103721135,291.823925943689,4.52836682984767));
#12819=CARTESIAN_POINT('Ctrl Pts',(-8.99122327230091,291.961425943689,2.44429792557732));
#12820=CARTESIAN_POINT('Ctrl Pts',(-9.,292.098925943689,0.0327551936972079));
#12821=CARTESIAN_POINT('Ctrl Pts',(-9.0087767276991,292.236425943689,-2.3787875381829));
#12822=CARTESIAN_POINT('Ctrl Pts',(-7.81060623090856,292.373925943689,-4.47163317015234));
#12823=CARTESIAN_POINT('Ctrl Pts',(-6.61243573411802,292.511425943689,-6.56447880212179));
#12824=CARTESIAN_POINT('Ctrl Pts',(-4.52836682984766,292.648925943689,-7.77785103721135));
#12825=CARTESIAN_POINT('Ctrl Pts',(-2.44429792557731,292.786425943689,-8.99122327230091));
#12826=CARTESIAN_POINT('Ctrl Pts',(-0.0327551936972084,292.923925943689,
-9.));
#12827=CARTESIAN_POINT('Ctrl Pts',(2.3787875381829,293.061425943689,-9.0087767276991));
#12828=CARTESIAN_POINT('Ctrl Pts',(4.47163317015234,293.198925943689,-7.81060623090856));
#12829=CARTESIAN_POINT('Ctrl Pts',(6.56447880212178,293.336425943689,-6.61243573411802));
#12830=CARTESIAN_POINT('Ctrl Pts',(7.77785103721135,293.473925943689,-4.52836682984767));
#12831=CARTESIAN_POINT('Ctrl Pts',(8.99122327230091,293.611425943689,-2.44429792557732));
#12832=CARTESIAN_POINT('Ctrl Pts',(9.,293.748925943689,-0.032755193697209));
#12833=CARTESIAN_POINT('Ctrl Pts',(9.0087767276991,293.886425943689,2.37878753818289));
#12834=CARTESIAN_POINT('Ctrl Pts',(7.81060623090856,294.023925943689,4.47163317015234));
#12835=CARTESIAN_POINT('Ctrl Pts',(6.61243573411802,294.161425943689,6.56447880212178));
#12836=CARTESIAN_POINT('Ctrl Pts',(4.52836682984767,294.298925943689,7.77785103721135));
#12837=CARTESIAN_POINT('Ctrl Pts',(2.44429792557732,294.436425943689,8.99122327230091));
#12838=CARTESIAN_POINT('Ctrl Pts',(0.0327551936972095,294.573925943689,
9.));
#12839=CARTESIAN_POINT('Ctrl Pts',(-2.37878753818289,294.711425943689,9.0087767276991));
#12840=CARTESIAN_POINT('Ctrl Pts',(-4.47163317015233,294.848925943689,7.81060623090856));
#12841=CARTESIAN_POINT('Ctrl Pts',(-6.56447880212178,294.986425943689,6.61243573411802));
#12842=CARTESIAN_POINT('Ctrl Pts',(-7.77785103721135,295.123925943689,4.52836682984767));
#12843=CARTESIAN_POINT('Ctrl Pts',(-8.99122327230091,295.261425943689,2.44429792557732));
#12844=CARTESIAN_POINT('Ctrl Pts',(-9.,295.398925943689,0.0327551936972079));
#12845=CARTESIAN_POINT('Ctrl Pts',(-9.0087767276991,295.536425943689,-2.3787875381829));
#12846=CARTESIAN_POINT('Ctrl Pts',(-7.81060623090856,295.673925943689,-4.47163317015234));
#12847=CARTESIAN_POINT('Ctrl Pts',(-6.61243573411802,295.811425943689,-6.56447880212179));
#12848=CARTESIAN_POINT('Ctrl Pts',(-4.52836682984766,295.948925943689,-7.77785103721135));
#12849=CARTESIAN_POINT('Ctrl Pts',(-2.44429792557731,296.086425943689,-8.99122327230091));
#12850=CARTESIAN_POINT('Ctrl Pts',(-0.0327551936972084,296.223925943689,
-9.));
#12851=CARTESIAN_POINT('Ctrl Pts',(2.3787875381829,296.361425943689,-9.0087767276991));
#12852=CARTESIAN_POINT('Ctrl Pts',(4.47163317015234,296.498925943689,-7.81060623090856));
#12853=CARTESIAN_POINT('Ctrl Pts',(6.56447880212178,296.636425943689,-6.61243573411802));
#12854=CARTESIAN_POINT('Ctrl Pts',(7.77785103721135,296.773925943689,-4.52836682984767));
#12855=CARTESIAN_POINT('Ctrl Pts',(8.99122327230091,296.911425943689,-2.44429792557732));
#12856=CARTESIAN_POINT('Ctrl Pts',(9.,297.048925943689,-0.032755193697209));
#12857=CARTESIAN_POINT('Ctrl Pts',(9.0087767276991,297.186425943689,2.37878753818289));
#12858=CARTESIAN_POINT('Ctrl Pts',(7.81060623090856,297.323925943689,4.47163317015234));
#12859=CARTESIAN_POINT('Ctrl Pts',(6.61243573411802,297.461425943689,6.56447880212178));
#12860=CARTESIAN_POINT('Ctrl Pts',(4.52836682984767,297.598925943689,7.77785103721135));
#12861=CARTESIAN_POINT('Ctrl Pts',(2.44429792557732,297.736425943689,8.99122327230091));
#12862=CARTESIAN_POINT('Ctrl Pts',(0.0327551936972095,297.873925943689,
9.));
#12863=CARTESIAN_POINT('Ctrl Pts',(-2.37878753818289,298.011425943689,9.0087767276991));
#12864=CARTESIAN_POINT('Ctrl Pts',(-4.47163317015233,298.148925943689,7.81060623090856));
#12865=CARTESIAN_POINT('Ctrl Pts',(-6.56447880212178,298.286425943689,6.61243573411802));
#12866=CARTESIAN_POINT('Ctrl Pts',(-7.77785103721135,298.423925943689,4.52836682984767));
#12867=CARTESIAN_POINT('Ctrl Pts',(-8.99122327230091,298.561425943689,2.44429792557732));
#12868=CARTESIAN_POINT('Ctrl Pts',(-9.,298.698925943689,0.0327551936972079));
#12869=CARTESIAN_POINT('Ctrl Pts',(-9.0087767276991,298.836425943689,-2.3787875381829));
#12870=CARTESIAN_POINT('Ctrl Pts',(-7.81060623090856,298.973925943689,-4.47163317015234));
#12871=CARTESIAN_POINT('Ctrl Pts',(-6.61243573411802,299.111425943689,-6.56447880212179));
#12872=CARTESIAN_POINT('Ctrl Pts',(-4.52836682984766,299.248925943689,-7.77785103721135));
#12873=CARTESIAN_POINT('Ctrl Pts',(-2.44429792557731,299.386425943689,-8.99122327230091));
#12874=CARTESIAN_POINT('Ctrl Pts',(-0.0327551936972084,299.523925943689,
-9.));
#12875=CARTESIAN_POINT('Ctrl Pts',(2.3787875381829,299.661425943689,-9.0087767276991));
#12876=CARTESIAN_POINT('Ctrl Pts',(4.47163317015234,299.798925943689,-7.81060623090856));
#12877=CARTESIAN_POINT('Ctrl Pts',(6.56447880212178,299.936425943689,-6.61243573411802));
#12878=CARTESIAN_POINT('Ctrl Pts',(7.77785103721135,300.073925943689,-4.52836682984767));
#12879=CARTESIAN_POINT('Ctrl Pts',(8.99122327230091,300.211425943689,-2.44429792557732));
#12880=CARTESIAN_POINT('Ctrl Pts',(9.,300.348925943689,-0.032755193697209));
#12881=CARTESIAN_POINT('Ctrl Pts',(9.0087767276991,300.486425943689,2.37878753818289));
#12882=CARTESIAN_POINT('Ctrl Pts',(7.81060623090856,300.623925943689,4.47163317015234));
#12883=CARTESIAN_POINT('Ctrl Pts',(6.61243573411802,300.761425943689,6.56447880212178));
#12884=CARTESIAN_POINT('Ctrl Pts',(4.52836682984767,300.898925943689,7.77785103721135));
#12885=CARTESIAN_POINT('Ctrl Pts',(2.44429792557732,301.036425943689,8.99122327230091));
#12886=CARTESIAN_POINT('Ctrl Pts',(0.0327551936972095,301.173925943689,
9.));
#12887=CARTESIAN_POINT('Ctrl Pts',(-2.37878753818289,301.311425943689,9.0087767276991));
#12888=CARTESIAN_POINT('Ctrl Pts',(-4.47163317015233,301.448925943689,7.81060623090856));
#12889=CARTESIAN_POINT('Ctrl Pts',(-6.56447880212178,301.586425943689,6.61243573411802));
#12890=CARTESIAN_POINT('Ctrl Pts',(-7.77785103721135,301.723925943689,4.52836682984767));
#12891=CARTESIAN_POINT('Ctrl Pts',(-8.99122327230091,301.861425943689,2.44429792557732));
#12892=CARTESIAN_POINT('Ctrl Pts',(-9.,301.998925943689,0.0327551936972079));
#12893=CARTESIAN_POINT('Ctrl Pts',(-9.0087767276991,302.136425943689,-2.3787875381829));
#12894=CARTESIAN_POINT('Ctrl Pts',(-7.81060623090856,302.273925943689,-4.47163317015234));
#12895=CARTESIAN_POINT('Ctrl Pts',(-6.61243573411802,302.411425943689,-6.56447880212179));
#12896=CARTESIAN_POINT('Ctrl Pts',(-4.52836682984766,302.548925943689,-7.77785103721135));
#12897=CARTESIAN_POINT('Ctrl Pts',(-2.44429792557731,302.686425943689,-8.99122327230091));
#12898=CARTESIAN_POINT('Ctrl Pts',(-0.0327551936972084,302.823925943689,
-9.));
#12899=CARTESIAN_POINT('Ctrl Pts',(2.3787875381829,302.961425943689,-9.0087767276991));
#12900=CARTESIAN_POINT('Ctrl Pts',(4.47163317015234,303.098925943689,-7.81060623090856));
#12901=CARTESIAN_POINT('Ctrl Pts',(6.56447880212178,303.236425943689,-6.61243573411802));
#12902=CARTESIAN_POINT('Ctrl Pts',(7.77785103721135,303.373925943689,-4.52836682984767));
#12903=CARTESIAN_POINT('Ctrl Pts',(8.99122327230091,303.511425943689,-2.44429792557732));
#12904=CARTESIAN_POINT('Ctrl Pts',(9.,303.648925943689,-0.032755193697209));
#12905=CARTESIAN_POINT('Ctrl Pts',(9.0087767276991,303.786425943689,2.37878753818289));
#12906=CARTESIAN_POINT('Ctrl Pts',(7.81060623090856,303.923925943689,4.47163317015234));
#12907=CARTESIAN_POINT('Ctrl Pts',(6.61243573411802,304.061425943689,6.56447880212178));
#12908=CARTESIAN_POINT('Ctrl Pts',(4.52836682984767,304.198925943689,7.77785103721135));
#12909=CARTESIAN_POINT('Ctrl Pts',(2.44429792557732,304.336425943689,8.99122327230091));
#12910=CARTESIAN_POINT('Ctrl Pts',(0.0327551936972095,304.473925943689,
9.));
#12911=CARTESIAN_POINT('Ctrl Pts',(-2.37878753818289,304.611425943689,9.0087767276991));
#12912=CARTESIAN_POINT('Ctrl Pts',(-4.47163317015233,304.748925943689,7.81060623090856));
#12913=CARTESIAN_POINT('Ctrl Pts',(-6.56447880212178,304.886425943689,6.61243573411802));
#12914=CARTESIAN_POINT('Ctrl Pts',(-7.77785103721135,305.023925943689,4.52836682984767));
#12915=CARTESIAN_POINT('Ctrl Pts',(-8.99122327230091,305.161425943689,2.44429792557732));
#12916=CARTESIAN_POINT('Ctrl Pts',(-9.,305.298925943689,0.0327551936972079));
#12917=CARTESIAN_POINT('Ctrl Pts',(-9.0087767276991,305.436425943689,-2.3787875381829));
#12918=CARTESIAN_POINT('Ctrl Pts',(-7.81060623090856,305.573925943689,-4.47163317015234));
#12919=CARTESIAN_POINT('Ctrl Pts',(-6.61243573411802,305.711425943689,-6.56447880212179));
#12920=CARTESIAN_POINT('Ctrl Pts',(-4.52836682984766,305.848925943689,-7.77785103721135));
#12921=CARTESIAN_POINT('Ctrl Pts',(-2.44429792557731,305.986425943689,-8.99122327230091));
#12922=CARTESIAN_POINT('Ctrl Pts',(-0.0327551936972084,306.123925943689,
-9.));
#12923=CARTESIAN_POINT('Ctrl Pts',(2.3787875381829,306.261425943689,-9.0087767276991));
#12924=CARTESIAN_POINT('Ctrl Pts',(4.47163317015234,306.398925943689,-7.81060623090856));
#12925=CARTESIAN_POINT('Ctrl Pts',(6.56447880212178,306.536425943689,-6.61243573411802));
#12926=CARTESIAN_POINT('Ctrl Pts',(7.77785103721135,306.673925943689,-4.52836682984767));
#12927=CARTESIAN_POINT('Ctrl Pts',(8.99122327230091,306.811425943689,-2.44429792557732));
#12928=CARTESIAN_POINT('Ctrl Pts',(9.,306.948925943689,-0.032755193697209));
#12929=CARTESIAN_POINT('Ctrl Pts',(9.0087767276991,307.086425943689,2.37878753818289));
#12930=CARTESIAN_POINT('Ctrl Pts',(7.81060623090856,307.223925943689,4.47163317015234));
#12931=CARTESIAN_POINT('Ctrl Pts',(6.61243573411802,307.361425943689,6.56447880212178));
#12932=CARTESIAN_POINT('Ctrl Pts',(4.52836682984767,307.498925943689,7.77785103721135));
#12933=CARTESIAN_POINT('Ctrl Pts',(2.44429792557732,307.636425943689,8.99122327230091));
#12934=CARTESIAN_POINT('Ctrl Pts',(0.0327551936972095,307.773925943689,
9.));
#12935=CARTESIAN_POINT('Ctrl Pts',(-2.37878753818289,307.911425943689,9.0087767276991));
#12936=CARTESIAN_POINT('Ctrl Pts',(-4.47163317015233,308.048925943689,7.81060623090856));
#12937=CARTESIAN_POINT('Ctrl Pts',(-6.56447880212178,308.186425943689,6.61243573411802));
#12938=CARTESIAN_POINT('Ctrl Pts',(-7.77785103721135,308.323925943689,4.52836682984767));
#12939=CARTESIAN_POINT('Ctrl Pts',(-8.99122327230091,308.461425943689,2.44429792557732));
#12940=CARTESIAN_POINT('Ctrl Pts',(-9.,308.598925943689,0.0327551936972079));
#12941=CARTESIAN_POINT('Ctrl Pts',(-9.0087767276991,308.736425943689,-2.3787875381829));
#12942=CARTESIAN_POINT('Ctrl Pts',(-7.81060623090856,308.873925943689,-4.47163317015234));
#12943=CARTESIAN_POINT('Ctrl Pts',(-6.61243573411802,309.011425943689,-6.56447880212179));
#12944=CARTESIAN_POINT('Ctrl Pts',(-4.52836682984766,309.148925943689,-7.77785103721135));
#12945=CARTESIAN_POINT('Ctrl Pts',(-2.44429792557731,309.286425943689,-8.99122327230091));
#12946=CARTESIAN_POINT('Ctrl Pts',(-0.0327551936972084,309.423925943689,
-9.));
#12947=CARTESIAN_POINT('Ctrl Pts',(2.3787875381829,309.561425943689,-9.0087767276991));
#12948=CARTESIAN_POINT('Ctrl Pts',(4.47163317015234,309.698925943689,-7.81060623090856));
#12949=CARTESIAN_POINT('Ctrl Pts',(6.56447880212178,309.836425943689,-6.61243573411802));
#12950=CARTESIAN_POINT('Ctrl Pts',(7.77785103721135,309.973925943689,-4.52836682984767));
#12951=CARTESIAN_POINT('Ctrl Pts',(8.99122327230091,310.111425943689,-2.44429792557732));
#12952=CARTESIAN_POINT('Ctrl Pts',(9.,310.248925943689,-0.032755193697209));
#12953=CARTESIAN_POINT('Ctrl Pts',(9.0087767276991,310.386425943689,2.37878753818289));
#12954=CARTESIAN_POINT('Ctrl Pts',(7.81060623090856,310.523925943689,4.47163317015234));
#12955=CARTESIAN_POINT('Ctrl Pts',(6.61243573411802,310.661425943689,6.56447880212178));
#12956=CARTESIAN_POINT('Ctrl Pts',(4.52836682984767,310.798925943689,7.77785103721135));
#12957=CARTESIAN_POINT('Ctrl Pts',(2.44429792557732,310.936425943689,8.99122327230091));
#12958=CARTESIAN_POINT('Ctrl Pts',(0.0327551936972095,311.073925943689,
9.));
#12959=CARTESIAN_POINT('Ctrl Pts',(-2.37878753818289,311.211425943689,9.0087767276991));
#12960=CARTESIAN_POINT('Ctrl Pts',(-4.47163317015233,311.348925943689,7.81060623090856));
#12961=CARTESIAN_POINT('Ctrl Pts',(-6.56447880212178,311.486425943689,6.61243573411802));
#12962=CARTESIAN_POINT('Ctrl Pts',(-7.77785103721135,311.623925943689,4.52836682984767));
#12963=CARTESIAN_POINT('Ctrl Pts',(-8.99122327230091,311.761425943689,2.44429792557732));
#12964=CARTESIAN_POINT('Ctrl Pts',(-9.,311.898925943689,0.0327551936972079));
#12965=CARTESIAN_POINT('Ctrl Pts',(-9.0087767276991,312.036425943689,-2.3787875381829));
#12966=CARTESIAN_POINT('Ctrl Pts',(-7.81060623090856,312.173925943689,-4.47163317015234));
#12967=CARTESIAN_POINT('Ctrl Pts',(-6.61243573411802,312.311425943689,-6.56447880212179));
#12968=CARTESIAN_POINT('Ctrl Pts',(-4.52836682984766,312.448925943689,-7.77785103721135));
#12969=CARTESIAN_POINT('Ctrl Pts',(-2.44429792557731,312.586425943689,-8.99122327230091));
#12970=CARTESIAN_POINT('Ctrl Pts',(-0.0327551936972084,312.723925943689,
-9.));
#12971=CARTESIAN_POINT('Ctrl Pts',(2.3787875381829,312.861425943689,-9.0087767276991));
#12972=CARTESIAN_POINT('Ctrl Pts',(4.47163317015234,312.998925943689,-7.81060623090856));
#12973=CARTESIAN_POINT('Ctrl Pts',(6.56447880212178,313.136425943689,-6.61243573411802));
#12974=CARTESIAN_POINT('Ctrl Pts',(7.77785103721135,313.273925943689,-4.52836682984767));
#12975=CARTESIAN_POINT('Ctrl Pts',(8.99122327230091,313.411425943689,-2.44429792557732));
#12976=CARTESIAN_POINT('Ctrl Pts',(9.,313.548925943689,-0.032755193697209));
#12977=CARTESIAN_POINT('Ctrl Pts',(9.0087767276991,313.686425943689,2.37878753818289));
#12978=CARTESIAN_POINT('Ctrl Pts',(7.81060623090856,313.823925943689,4.47163317015234));
#12979=CARTESIAN_POINT('Ctrl Pts',(6.61243573411802,313.961425943689,6.56447880212178));
#12980=CARTESIAN_POINT('Ctrl Pts',(4.52836682984767,314.098925943689,7.77785103721135));
#12981=CARTESIAN_POINT('Ctrl Pts',(2.44429792557732,314.236425943689,8.99122327230091));
#12982=CARTESIAN_POINT('Ctrl Pts',(0.0327551936972095,314.373925943689,
9.));
#12983=CARTESIAN_POINT('Ctrl Pts',(-2.37878753818289,314.511425943689,9.0087767276991));
#12984=CARTESIAN_POINT('Ctrl Pts',(-4.47163317015233,314.648925943689,7.81060623090856));
#12985=CARTESIAN_POINT('Ctrl Pts',(-6.56447880212178,314.786425943689,6.61243573411802));
#12986=CARTESIAN_POINT('Ctrl Pts',(-7.77785103721135,314.923925943689,4.52836682984767));
#12987=CARTESIAN_POINT('Ctrl Pts',(-8.99122327230091,315.061425943689,2.44429792557732));
#12988=CARTESIAN_POINT('Ctrl Pts',(-9.,315.198925943689,0.0327551936972079));
#12989=CARTESIAN_POINT('Ctrl Pts',(-9.0087767276991,315.336425943689,-2.3787875381829));
#12990=CARTESIAN_POINT('Ctrl Pts',(-7.81060623090856,315.473925943689,-4.47163317015234));
#12991=CARTESIAN_POINT('Ctrl Pts',(-6.61243573411802,315.611425943689,-6.56447880212179));
#12992=CARTESIAN_POINT('Ctrl Pts',(-4.52836682984766,315.748925943689,-7.77785103721135));
#12993=CARTESIAN_POINT('Ctrl Pts',(-2.44429792557731,315.886425943689,-8.99122327230091));
#12994=CARTESIAN_POINT('Ctrl Pts',(-0.0327551936972084,316.023925943689,
-9.));
#12995=CARTESIAN_POINT('Ctrl Pts',(2.3787875381829,316.161425943689,-9.0087767276991));
#12996=CARTESIAN_POINT('Ctrl Pts',(4.47163317015234,316.298925943689,-7.81060623090856));
#12997=CARTESIAN_POINT('Ctrl Pts',(6.56447880212178,316.436425943689,-6.61243573411802));
#12998=CARTESIAN_POINT('Ctrl Pts',(7.77785103721135,316.573925943689,-4.52836682984767));
#12999=CARTESIAN_POINT('Ctrl Pts',(8.99122327230091,316.711425943689,-2.44429792557732));
#13000=CARTESIAN_POINT('Ctrl Pts',(9.,316.848925943689,-0.032755193697209));
#13001=CARTESIAN_POINT('Ctrl Pts',(9.0087767276991,316.986425943689,2.37878753818289));
#13002=CARTESIAN_POINT('Ctrl Pts',(7.81060623090856,317.123925943689,4.47163317015234));
#13003=CARTESIAN_POINT('Ctrl Pts',(6.61243573411802,317.261425943689,6.56447880212178));
#13004=CARTESIAN_POINT('Ctrl Pts',(4.52836682984767,317.398925943689,7.77785103721135));
#13005=CARTESIAN_POINT('Ctrl Pts',(2.44429792557732,317.536425943689,8.99122327230091));
#13006=CARTESIAN_POINT('Ctrl Pts',(0.0327551936972095,317.673925943689,
9.));
#13007=CARTESIAN_POINT('Ctrl Pts',(-2.37878753818289,317.811425943689,9.0087767276991));
#13008=CARTESIAN_POINT('Ctrl Pts',(-4.47163317015233,317.948925943689,7.81060623090856));
#13009=CARTESIAN_POINT('Ctrl Pts',(-6.56447880212178,318.086425943689,6.61243573411802));
#13010=CARTESIAN_POINT('Ctrl Pts',(-7.77785103721135,318.223925943689,4.52836682984767));
#13011=CARTESIAN_POINT('Ctrl Pts',(-8.99122327230091,318.361425943689,2.44429792557732));
#13012=CARTESIAN_POINT('Ctrl Pts',(-9.,318.498925943689,0.0327551936972079));
#13013=CARTESIAN_POINT('Ctrl Pts',(-8.,285.498925943689,0.0327551936971979));
#13014=CARTESIAN_POINT('Ctrl Pts',(-8.00877672769909,285.636425943689,-2.11083834575178));
#13015=CARTESIAN_POINT('Ctrl Pts',(-6.94458082712411,285.773925943689,-3.97163317015235));
#13016=CARTESIAN_POINT('Ctrl Pts',(-5.88038492654913,285.911425943689,-5.83242799455291));
#13017=CARTESIAN_POINT('Ctrl Pts',(-4.02836682984766,286.048925943689,-6.91182563342691));
#13018=CARTESIAN_POINT('Ctrl Pts',(-2.17634873314618,286.186425943689,-7.99122327230091));
#13019=CARTESIAN_POINT('Ctrl Pts',(-0.0327551936971984,286.323925943689,
-8.));
#13020=CARTESIAN_POINT('Ctrl Pts',(2.11083834575178,286.461425943689,-8.00877672769909));
#13021=CARTESIAN_POINT('Ctrl Pts',(3.97163317015235,286.598925943689,-6.94458082712411));
#13022=CARTESIAN_POINT('Ctrl Pts',(5.83242799455291,286.736425943689,-5.88038492654913));
#13023=CARTESIAN_POINT('Ctrl Pts',(6.91182563342691,286.873925943689,-4.02836682984766));
#13024=CARTESIAN_POINT('Ctrl Pts',(7.99122327230091,287.011425943689,-2.17634873314618));
#13025=CARTESIAN_POINT('Ctrl Pts',(8.,287.148925943689,-0.0327551936971989));
#13026=CARTESIAN_POINT('Ctrl Pts',(8.00877672769909,287.286425943689,2.11083834575178));
#13027=CARTESIAN_POINT('Ctrl Pts',(6.94458082712411,287.423925943689,3.97163317015235));
#13028=CARTESIAN_POINT('Ctrl Pts',(5.88038492654913,287.561425943689,5.83242799455291));
#13029=CARTESIAN_POINT('Ctrl Pts',(4.02836682984766,287.698925943689,6.91182563342691));
#13030=CARTESIAN_POINT('Ctrl Pts',(2.17634873314619,287.836425943689,7.99122327230091));
#13031=CARTESIAN_POINT('Ctrl Pts',(0.0327551936971994,287.973925943689,
8.));
#13032=CARTESIAN_POINT('Ctrl Pts',(-2.11083834575178,288.111425943689,8.00877672769909));
#13033=CARTESIAN_POINT('Ctrl Pts',(-3.97163317015234,288.248925943689,6.94458082712412));
#13034=CARTESIAN_POINT('Ctrl Pts',(-5.83242799455291,288.386425943689,5.88038492654913));
#13035=CARTESIAN_POINT('Ctrl Pts',(-6.91182563342691,288.523925943689,4.02836682984766));
#13036=CARTESIAN_POINT('Ctrl Pts',(-7.99122327230091,288.661425943689,2.17634873314619));
#13037=CARTESIAN_POINT('Ctrl Pts',(-8.,288.798925943689,0.0327551936971979));
#13038=CARTESIAN_POINT('Ctrl Pts',(-8.00877672769909,288.936425943689,-2.11083834575178));
#13039=CARTESIAN_POINT('Ctrl Pts',(-6.94458082712411,289.073925943689,-3.97163317015235));
#13040=CARTESIAN_POINT('Ctrl Pts',(-5.88038492654913,289.211425943689,-5.83242799455291));
#13041=CARTESIAN_POINT('Ctrl Pts',(-4.02836682984766,289.348925943689,-6.91182563342691));
#13042=CARTESIAN_POINT('Ctrl Pts',(-2.17634873314618,289.486425943689,-7.99122327230091));
#13043=CARTESIAN_POINT('Ctrl Pts',(-0.0327551936971984,289.623925943689,
-8.));
#13044=CARTESIAN_POINT('Ctrl Pts',(2.11083834575178,289.761425943689,-8.00877672769909));
#13045=CARTESIAN_POINT('Ctrl Pts',(3.97163317015235,289.898925943689,-6.94458082712411));
#13046=CARTESIAN_POINT('Ctrl Pts',(5.83242799455291,290.036425943689,-5.88038492654913));
#13047=CARTESIAN_POINT('Ctrl Pts',(6.91182563342691,290.173925943689,-4.02836682984766));
#13048=CARTESIAN_POINT('Ctrl Pts',(7.99122327230091,290.311425943689,-2.17634873314618));
#13049=CARTESIAN_POINT('Ctrl Pts',(8.,290.448925943689,-0.0327551936971989));
#13050=CARTESIAN_POINT('Ctrl Pts',(8.00877672769909,290.586425943689,2.11083834575178));
#13051=CARTESIAN_POINT('Ctrl Pts',(6.94458082712411,290.723925943689,3.97163317015235));
#13052=CARTESIAN_POINT('Ctrl Pts',(5.88038492654913,290.861425943689,5.83242799455291));
#13053=CARTESIAN_POINT('Ctrl Pts',(4.02836682984766,290.998925943689,6.91182563342691));
#13054=CARTESIAN_POINT('Ctrl Pts',(2.17634873314619,291.136425943689,7.99122327230091));
#13055=CARTESIAN_POINT('Ctrl Pts',(0.0327551936971994,291.273925943689,
8.));
#13056=CARTESIAN_POINT('Ctrl Pts',(-2.11083834575178,291.411425943689,8.00877672769909));
#13057=CARTESIAN_POINT('Ctrl Pts',(-3.97163317015234,291.548925943689,6.94458082712412));
#13058=CARTESIAN_POINT('Ctrl Pts',(-5.83242799455291,291.686425943689,5.88038492654913));
#13059=CARTESIAN_POINT('Ctrl Pts',(-6.91182563342691,291.823925943689,4.02836682984766));
#13060=CARTESIAN_POINT('Ctrl Pts',(-7.99122327230091,291.961425943689,2.17634873314619));
#13061=CARTESIAN_POINT('Ctrl Pts',(-8.,292.098925943689,0.0327551936971979));
#13062=CARTESIAN_POINT('Ctrl Pts',(-8.00877672769909,292.236425943689,-2.11083834575178));
#13063=CARTESIAN_POINT('Ctrl Pts',(-6.94458082712411,292.373925943689,-3.97163317015235));
#13064=CARTESIAN_POINT('Ctrl Pts',(-5.88038492654913,292.511425943689,-5.83242799455291));
#13065=CARTESIAN_POINT('Ctrl Pts',(-4.02836682984766,292.648925943689,-6.91182563342691));
#13066=CARTESIAN_POINT('Ctrl Pts',(-2.17634873314618,292.786425943689,-7.99122327230091));
#13067=CARTESIAN_POINT('Ctrl Pts',(-0.0327551936971984,292.923925943689,
-8.));
#13068=CARTESIAN_POINT('Ctrl Pts',(2.11083834575178,293.061425943689,-8.00877672769909));
#13069=CARTESIAN_POINT('Ctrl Pts',(3.97163317015235,293.198925943689,-6.94458082712411));
#13070=CARTESIAN_POINT('Ctrl Pts',(5.83242799455291,293.336425943689,-5.88038492654913));
#13071=CARTESIAN_POINT('Ctrl Pts',(6.91182563342691,293.473925943689,-4.02836682984766));
#13072=CARTESIAN_POINT('Ctrl Pts',(7.99122327230091,293.611425943689,-2.17634873314618));
#13073=CARTESIAN_POINT('Ctrl Pts',(8.,293.748925943689,-0.0327551936971989));
#13074=CARTESIAN_POINT('Ctrl Pts',(8.00877672769909,293.886425943689,2.11083834575178));
#13075=CARTESIAN_POINT('Ctrl Pts',(6.94458082712411,294.023925943689,3.97163317015235));
#13076=CARTESIAN_POINT('Ctrl Pts',(5.88038492654913,294.161425943689,5.83242799455291));
#13077=CARTESIAN_POINT('Ctrl Pts',(4.02836682984766,294.298925943689,6.91182563342691));
#13078=CARTESIAN_POINT('Ctrl Pts',(2.17634873314619,294.436425943689,7.99122327230091));
#13079=CARTESIAN_POINT('Ctrl Pts',(0.0327551936971994,294.573925943689,
8.));
#13080=CARTESIAN_POINT('Ctrl Pts',(-2.11083834575178,294.711425943689,8.00877672769909));
#13081=CARTESIAN_POINT('Ctrl Pts',(-3.97163317015234,294.848925943689,6.94458082712412));
#13082=CARTESIAN_POINT('Ctrl Pts',(-5.83242799455291,294.986425943689,5.88038492654913));
#13083=CARTESIAN_POINT('Ctrl Pts',(-6.91182563342691,295.123925943689,4.02836682984766));
#13084=CARTESIAN_POINT('Ctrl Pts',(-7.99122327230091,295.261425943689,2.17634873314619));
#13085=CARTESIAN_POINT('Ctrl Pts',(-8.,295.398925943689,0.0327551936971979));
#13086=CARTESIAN_POINT('Ctrl Pts',(-8.00877672769909,295.536425943689,-2.11083834575178));
#13087=CARTESIAN_POINT('Ctrl Pts',(-6.94458082712411,295.673925943689,-3.97163317015235));
#13088=CARTESIAN_POINT('Ctrl Pts',(-5.88038492654913,295.811425943689,-5.83242799455291));
#13089=CARTESIAN_POINT('Ctrl Pts',(-4.02836682984766,295.948925943689,-6.91182563342691));
#13090=CARTESIAN_POINT('Ctrl Pts',(-2.17634873314618,296.086425943689,-7.99122327230091));
#13091=CARTESIAN_POINT('Ctrl Pts',(-0.0327551936971984,296.223925943689,
-8.));
#13092=CARTESIAN_POINT('Ctrl Pts',(2.11083834575178,296.361425943689,-8.00877672769909));
#13093=CARTESIAN_POINT('Ctrl Pts',(3.97163317015235,296.498925943689,-6.94458082712411));
#13094=CARTESIAN_POINT('Ctrl Pts',(5.83242799455291,296.636425943689,-5.88038492654913));
#13095=CARTESIAN_POINT('Ctrl Pts',(6.91182563342691,296.773925943689,-4.02836682984766));
#13096=CARTESIAN_POINT('Ctrl Pts',(7.99122327230091,296.911425943689,-2.17634873314618));
#13097=CARTESIAN_POINT('Ctrl Pts',(8.,297.048925943689,-0.0327551936971989));
#13098=CARTESIAN_POINT('Ctrl Pts',(8.00877672769909,297.186425943689,2.11083834575178));
#13099=CARTESIAN_POINT('Ctrl Pts',(6.94458082712411,297.323925943689,3.97163317015235));
#13100=CARTESIAN_POINT('Ctrl Pts',(5.88038492654913,297.461425943689,5.83242799455291));
#13101=CARTESIAN_POINT('Ctrl Pts',(4.02836682984766,297.598925943689,6.91182563342691));
#13102=CARTESIAN_POINT('Ctrl Pts',(2.17634873314619,297.736425943689,7.99122327230091));
#13103=CARTESIAN_POINT('Ctrl Pts',(0.0327551936971994,297.873925943689,
8.));
#13104=CARTESIAN_POINT('Ctrl Pts',(-2.11083834575178,298.011425943689,8.00877672769909));
#13105=CARTESIAN_POINT('Ctrl Pts',(-3.97163317015234,298.148925943689,6.94458082712412));
#13106=CARTESIAN_POINT('Ctrl Pts',(-5.83242799455291,298.286425943689,5.88038492654913));
#13107=CARTESIAN_POINT('Ctrl Pts',(-6.91182563342691,298.423925943689,4.02836682984766));
#13108=CARTESIAN_POINT('Ctrl Pts',(-7.99122327230091,298.561425943689,2.17634873314619));
#13109=CARTESIAN_POINT('Ctrl Pts',(-8.,298.698925943689,0.0327551936971979));
#13110=CARTESIAN_POINT('Ctrl Pts',(-8.00877672769909,298.836425943689,-2.11083834575178));
#13111=CARTESIAN_POINT('Ctrl Pts',(-6.94458082712411,298.973925943689,-3.97163317015235));
#13112=CARTESIAN_POINT('Ctrl Pts',(-5.88038492654913,299.111425943689,-5.83242799455291));
#13113=CARTESIAN_POINT('Ctrl Pts',(-4.02836682984766,299.248925943689,-6.91182563342691));
#13114=CARTESIAN_POINT('Ctrl Pts',(-2.17634873314618,299.386425943689,-7.99122327230091));
#13115=CARTESIAN_POINT('Ctrl Pts',(-0.0327551936971984,299.523925943689,
-8.));
#13116=CARTESIAN_POINT('Ctrl Pts',(2.11083834575178,299.661425943689,-8.00877672769909));
#13117=CARTESIAN_POINT('Ctrl Pts',(3.97163317015235,299.798925943689,-6.94458082712411));
#13118=CARTESIAN_POINT('Ctrl Pts',(5.83242799455291,299.936425943689,-5.88038492654913));
#13119=CARTESIAN_POINT('Ctrl Pts',(6.91182563342691,300.073925943689,-4.02836682984766));
#13120=CARTESIAN_POINT('Ctrl Pts',(7.99122327230091,300.211425943689,-2.17634873314618));
#13121=CARTESIAN_POINT('Ctrl Pts',(8.,300.348925943689,-0.0327551936971989));
#13122=CARTESIAN_POINT('Ctrl Pts',(8.00877672769909,300.486425943689,2.11083834575178));
#13123=CARTESIAN_POINT('Ctrl Pts',(6.94458082712411,300.623925943689,3.97163317015235));
#13124=CARTESIAN_POINT('Ctrl Pts',(5.88038492654913,300.761425943689,5.83242799455291));
#13125=CARTESIAN_POINT('Ctrl Pts',(4.02836682984766,300.898925943689,6.91182563342691));
#13126=CARTESIAN_POINT('Ctrl Pts',(2.17634873314619,301.036425943689,7.99122327230091));
#13127=CARTESIAN_POINT('Ctrl Pts',(0.0327551936971994,301.173925943689,
8.));
#13128=CARTESIAN_POINT('Ctrl Pts',(-2.11083834575178,301.311425943689,8.00877672769909));
#13129=CARTESIAN_POINT('Ctrl Pts',(-3.97163317015234,301.448925943689,6.94458082712412));
#13130=CARTESIAN_POINT('Ctrl Pts',(-5.83242799455291,301.586425943689,5.88038492654913));
#13131=CARTESIAN_POINT('Ctrl Pts',(-6.91182563342691,301.723925943689,4.02836682984766));
#13132=CARTESIAN_POINT('Ctrl Pts',(-7.99122327230091,301.861425943689,2.17634873314619));
#13133=CARTESIAN_POINT('Ctrl Pts',(-8.,301.998925943689,0.0327551936971979));
#13134=CARTESIAN_POINT('Ctrl Pts',(-8.00877672769909,302.136425943689,-2.11083834575178));
#13135=CARTESIAN_POINT('Ctrl Pts',(-6.94458082712411,302.273925943689,-3.97163317015235));
#13136=CARTESIAN_POINT('Ctrl Pts',(-5.88038492654913,302.411425943689,-5.83242799455291));
#13137=CARTESIAN_POINT('Ctrl Pts',(-4.02836682984766,302.548925943689,-6.91182563342691));
#13138=CARTESIAN_POINT('Ctrl Pts',(-2.17634873314618,302.686425943689,-7.99122327230091));
#13139=CARTESIAN_POINT('Ctrl Pts',(-0.0327551936971984,302.823925943689,
-8.));
#13140=CARTESIAN_POINT('Ctrl Pts',(2.11083834575178,302.961425943689,-8.00877672769909));
#13141=CARTESIAN_POINT('Ctrl Pts',(3.97163317015235,303.098925943689,-6.94458082712411));
#13142=CARTESIAN_POINT('Ctrl Pts',(5.83242799455291,303.236425943689,-5.88038492654913));
#13143=CARTESIAN_POINT('Ctrl Pts',(6.91182563342691,303.373925943689,-4.02836682984766));
#13144=CARTESIAN_POINT('Ctrl Pts',(7.99122327230091,303.511425943689,-2.17634873314618));
#13145=CARTESIAN_POINT('Ctrl Pts',(8.,303.648925943689,-0.0327551936971989));
#13146=CARTESIAN_POINT('Ctrl Pts',(8.00877672769909,303.786425943689,2.11083834575178));
#13147=CARTESIAN_POINT('Ctrl Pts',(6.94458082712411,303.923925943689,3.97163317015235));
#13148=CARTESIAN_POINT('Ctrl Pts',(5.88038492654913,304.061425943689,5.83242799455291));
#13149=CARTESIAN_POINT('Ctrl Pts',(4.02836682984766,304.198925943689,6.91182563342691));
#13150=CARTESIAN_POINT('Ctrl Pts',(2.17634873314619,304.336425943689,7.99122327230091));
#13151=CARTESIAN_POINT('Ctrl Pts',(0.0327551936971994,304.473925943689,
8.));
#13152=CARTESIAN_POINT('Ctrl Pts',(-2.11083834575178,304.611425943689,8.00877672769909));
#13153=CARTESIAN_POINT('Ctrl Pts',(-3.97163317015234,304.748925943689,6.94458082712412));
#13154=CARTESIAN_POINT('Ctrl Pts',(-5.83242799455291,304.886425943689,5.88038492654913));
#13155=CARTESIAN_POINT('Ctrl Pts',(-6.91182563342691,305.023925943689,4.02836682984766));
#13156=CARTESIAN_POINT('Ctrl Pts',(-7.99122327230091,305.161425943689,2.17634873314619));
#13157=CARTESIAN_POINT('Ctrl Pts',(-8.,305.298925943689,0.0327551936971979));
#13158=CARTESIAN_POINT('Ctrl Pts',(-8.00877672769909,305.436425943689,-2.11083834575178));
#13159=CARTESIAN_POINT('Ctrl Pts',(-6.94458082712411,305.573925943689,-3.97163317015235));
#13160=CARTESIAN_POINT('Ctrl Pts',(-5.88038492654913,305.711425943689,-5.83242799455291));
#13161=CARTESIAN_POINT('Ctrl Pts',(-4.02836682984766,305.848925943689,-6.91182563342691));
#13162=CARTESIAN_POINT('Ctrl Pts',(-2.17634873314618,305.986425943689,-7.99122327230091));
#13163=CARTESIAN_POINT('Ctrl Pts',(-0.0327551936971984,306.123925943689,
-8.));
#13164=CARTESIAN_POINT('Ctrl Pts',(2.11083834575178,306.261425943689,-8.00877672769909));
#13165=CARTESIAN_POINT('Ctrl Pts',(3.97163317015235,306.398925943689,-6.94458082712411));
#13166=CARTESIAN_POINT('Ctrl Pts',(5.83242799455291,306.536425943689,-5.88038492654913));
#13167=CARTESIAN_POINT('Ctrl Pts',(6.91182563342691,306.673925943689,-4.02836682984766));
#13168=CARTESIAN_POINT('Ctrl Pts',(7.99122327230091,306.811425943689,-2.17634873314618));
#13169=CARTESIAN_POINT('Ctrl Pts',(8.,306.948925943689,-0.0327551936971989));
#13170=CARTESIAN_POINT('Ctrl Pts',(8.00877672769909,307.086425943689,2.11083834575178));
#13171=CARTESIAN_POINT('Ctrl Pts',(6.94458082712411,307.223925943689,3.97163317015235));
#13172=CARTESIAN_POINT('Ctrl Pts',(5.88038492654913,307.361425943689,5.83242799455291));
#13173=CARTESIAN_POINT('Ctrl Pts',(4.02836682984766,307.498925943689,6.91182563342691));
#13174=CARTESIAN_POINT('Ctrl Pts',(2.17634873314619,307.636425943689,7.99122327230091));
#13175=CARTESIAN_POINT('Ctrl Pts',(0.0327551936971994,307.773925943689,
8.));
#13176=CARTESIAN_POINT('Ctrl Pts',(-2.11083834575178,307.911425943689,8.00877672769909));
#13177=CARTESIAN_POINT('Ctrl Pts',(-3.97163317015234,308.048925943689,6.94458082712412));
#13178=CARTESIAN_POINT('Ctrl Pts',(-5.83242799455291,308.186425943689,5.88038492654913));
#13179=CARTESIAN_POINT('Ctrl Pts',(-6.91182563342691,308.323925943689,4.02836682984766));
#13180=CARTESIAN_POINT('Ctrl Pts',(-7.99122327230091,308.461425943689,2.17634873314619));
#13181=CARTESIAN_POINT('Ctrl Pts',(-8.,308.598925943689,0.0327551936971979));
#13182=CARTESIAN_POINT('Ctrl Pts',(-8.00877672769909,308.736425943689,-2.11083834575178));
#13183=CARTESIAN_POINT('Ctrl Pts',(-6.94458082712411,308.873925943689,-3.97163317015235));
#13184=CARTESIAN_POINT('Ctrl Pts',(-5.88038492654913,309.011425943689,-5.83242799455291));
#13185=CARTESIAN_POINT('Ctrl Pts',(-4.02836682984766,309.148925943689,-6.91182563342691));
#13186=CARTESIAN_POINT('Ctrl Pts',(-2.17634873314618,309.286425943689,-7.99122327230091));
#13187=CARTESIAN_POINT('Ctrl Pts',(-0.0327551936971984,309.423925943689,
-8.));
#13188=CARTESIAN_POINT('Ctrl Pts',(2.11083834575178,309.561425943689,-8.00877672769909));
#13189=CARTESIAN_POINT('Ctrl Pts',(3.97163317015235,309.698925943689,-6.94458082712411));
#13190=CARTESIAN_POINT('Ctrl Pts',(5.83242799455291,309.836425943689,-5.88038492654913));
#13191=CARTESIAN_POINT('Ctrl Pts',(6.91182563342691,309.973925943689,-4.02836682984766));
#13192=CARTESIAN_POINT('Ctrl Pts',(7.99122327230091,310.111425943689,-2.17634873314618));
#13193=CARTESIAN_POINT('Ctrl Pts',(8.,310.248925943689,-0.0327551936971989));
#13194=CARTESIAN_POINT('Ctrl Pts',(8.00877672769909,310.386425943689,2.11083834575178));
#13195=CARTESIAN_POINT('Ctrl Pts',(6.94458082712411,310.523925943689,3.97163317015235));
#13196=CARTESIAN_POINT('Ctrl Pts',(5.88038492654913,310.661425943689,5.83242799455291));
#13197=CARTESIAN_POINT('Ctrl Pts',(4.02836682984766,310.798925943689,6.91182563342691));
#13198=CARTESIAN_POINT('Ctrl Pts',(2.17634873314619,310.936425943689,7.99122327230091));
#13199=CARTESIAN_POINT('Ctrl Pts',(0.0327551936971994,311.073925943689,
8.));
#13200=CARTESIAN_POINT('Ctrl Pts',(-2.11083834575178,311.211425943689,8.00877672769909));
#13201=CARTESIAN_POINT('Ctrl Pts',(-3.97163317015234,311.348925943689,6.94458082712412));
#13202=CARTESIAN_POINT('Ctrl Pts',(-5.83242799455291,311.486425943689,5.88038492654913));
#13203=CARTESIAN_POINT('Ctrl Pts',(-6.91182563342691,311.623925943689,4.02836682984766));
#13204=CARTESIAN_POINT('Ctrl Pts',(-7.99122327230091,311.761425943689,2.17634873314619));
#13205=CARTESIAN_POINT('Ctrl Pts',(-8.,311.898925943689,0.0327551936971979));
#13206=CARTESIAN_POINT('Ctrl Pts',(-8.00877672769909,312.036425943689,-2.11083834575178));
#13207=CARTESIAN_POINT('Ctrl Pts',(-6.94458082712411,312.173925943689,-3.97163317015235));
#13208=CARTESIAN_POINT('Ctrl Pts',(-5.88038492654913,312.311425943689,-5.83242799455291));
#13209=CARTESIAN_POINT('Ctrl Pts',(-4.02836682984766,312.448925943689,-6.91182563342691));
#13210=CARTESIAN_POINT('Ctrl Pts',(-2.17634873314618,312.586425943689,-7.99122327230091));
#13211=CARTESIAN_POINT('Ctrl Pts',(-0.0327551936971984,312.723925943689,
-8.));
#13212=CARTESIAN_POINT('Ctrl Pts',(2.11083834575178,312.861425943689,-8.00877672769909));
#13213=CARTESIAN_POINT('Ctrl Pts',(3.97163317015235,312.998925943689,-6.94458082712411));
#13214=CARTESIAN_POINT('Ctrl Pts',(5.83242799455291,313.136425943689,-5.88038492654913));
#13215=CARTESIAN_POINT('Ctrl Pts',(6.91182563342691,313.273925943689,-4.02836682984766));
#13216=CARTESIAN_POINT('Ctrl Pts',(7.99122327230091,313.411425943689,-2.17634873314618));
#13217=CARTESIAN_POINT('Ctrl Pts',(8.,313.548925943689,-0.0327551936971989));
#13218=CARTESIAN_POINT('Ctrl Pts',(8.00877672769909,313.686425943689,2.11083834575178));
#13219=CARTESIAN_POINT('Ctrl Pts',(6.94458082712411,313.823925943689,3.97163317015235));
#13220=CARTESIAN_POINT('Ctrl Pts',(5.88038492654913,313.961425943689,5.83242799455291));
#13221=CARTESIAN_POINT('Ctrl Pts',(4.02836682984766,314.098925943689,6.91182563342691));
#13222=CARTESIAN_POINT('Ctrl Pts',(2.17634873314619,314.236425943689,7.99122327230091));
#13223=CARTESIAN_POINT('Ctrl Pts',(0.0327551936971994,314.373925943689,
8.));
#13224=CARTESIAN_POINT('Ctrl Pts',(-2.11083834575178,314.511425943689,8.00877672769909));
#13225=CARTESIAN_POINT('Ctrl Pts',(-3.97163317015234,314.648925943689,6.94458082712412));
#13226=CARTESIAN_POINT('Ctrl Pts',(-5.83242799455291,314.786425943689,5.88038492654913));
#13227=CARTESIAN_POINT('Ctrl Pts',(-6.91182563342691,314.923925943689,4.02836682984766));
#13228=CARTESIAN_POINT('Ctrl Pts',(-7.99122327230091,315.061425943689,2.17634873314619));
#13229=CARTESIAN_POINT('Ctrl Pts',(-8.,315.198925943689,0.0327551936971979));
#13230=CARTESIAN_POINT('Ctrl Pts',(-8.00877672769909,315.336425943689,-2.11083834575178));
#13231=CARTESIAN_POINT('Ctrl Pts',(-6.94458082712411,315.473925943689,-3.97163317015235));
#13232=CARTESIAN_POINT('Ctrl Pts',(-5.88038492654913,315.611425943689,-5.83242799455291));
#13233=CARTESIAN_POINT('Ctrl Pts',(-4.02836682984766,315.748925943689,-6.91182563342691));
#13234=CARTESIAN_POINT('Ctrl Pts',(-2.17634873314618,315.886425943689,-7.99122327230091));
#13235=CARTESIAN_POINT('Ctrl Pts',(-0.0327551936971984,316.023925943689,
-8.));
#13236=CARTESIAN_POINT('Ctrl Pts',(2.11083834575178,316.161425943689,-8.00877672769909));
#13237=CARTESIAN_POINT('Ctrl Pts',(3.97163317015235,316.298925943689,-6.94458082712411));
#13238=CARTESIAN_POINT('Ctrl Pts',(5.83242799455291,316.436425943689,-5.88038492654913));
#13239=CARTESIAN_POINT('Ctrl Pts',(6.91182563342691,316.573925943689,-4.02836682984766));
#13240=CARTESIAN_POINT('Ctrl Pts',(7.99122327230091,316.711425943689,-2.17634873314618));
#13241=CARTESIAN_POINT('Ctrl Pts',(8.,316.848925943689,-0.0327551936971989));
#13242=CARTESIAN_POINT('Ctrl Pts',(8.00877672769909,316.986425943689,2.11083834575178));
#13243=CARTESIAN_POINT('Ctrl Pts',(6.94458082712411,317.123925943689,3.97163317015235));
#13244=CARTESIAN_POINT('Ctrl Pts',(5.88038492654913,317.261425943689,5.83242799455291));
#13245=CARTESIAN_POINT('Ctrl Pts',(4.02836682984766,317.398925943689,6.91182563342691));
#13246=CARTESIAN_POINT('Ctrl Pts',(2.17634873314619,317.536425943689,7.99122327230091));
#13247=CARTESIAN_POINT('Ctrl Pts',(0.0327551936971994,317.673925943689,
8.));
#13248=CARTESIAN_POINT('Ctrl Pts',(-2.11083834575178,317.811425943689,8.00877672769909));
#13249=CARTESIAN_POINT('Ctrl Pts',(-3.97163317015234,317.948925943689,6.94458082712412));
#13250=CARTESIAN_POINT('Ctrl Pts',(-5.83242799455291,318.086425943689,5.88038492654913));
#13251=CARTESIAN_POINT('Ctrl Pts',(-6.91182563342691,318.223925943689,4.02836682984766));
#13252=CARTESIAN_POINT('Ctrl Pts',(-7.99122327230091,318.361425943689,2.17634873314619));
#13253=CARTESIAN_POINT('Ctrl Pts',(-8.,318.498925943689,0.0327551936971979));
#13254=CARTESIAN_POINT('Ctrl Pts',(-4.63461213585364,285.,-6.52084682023068));
#13255=CARTESIAN_POINT('Ctrl Pts',(-4.63617687809023,285.,-6.52302941473603));
#13256=CARTESIAN_POINT('Ctrl Pts',(-4.63798167723247,285.,-6.52498169175354));
#13257=CARTESIAN_POINT('Ctrl Pts',(-4.64219825050599,285.,-6.52861106616703));
#13258=CARTESIAN_POINT('Ctrl Pts',(-4.64459104103043,285.,-6.53021023836018));
#13259=CARTESIAN_POINT('Ctrl Pts',(-4.65315442170252,285.,-6.53481267652416));
#13260=CARTESIAN_POINT('Ctrl Pts',(-4.6600128556107,285.,-6.53672564774018));
#13261=CARTESIAN_POINT('Ctrl Pts',(-4.68576001867322,285.,-6.54097523595292));
#13262=CARTESIAN_POINT('Ctrl Pts',(-4.70898798502752,285.,-6.53862241186785));
#13263=CARTESIAN_POINT('Ctrl Pts',(-4.78979719606241,285.,-6.52397532465739));
#13264=CARTESIAN_POINT('Ctrl Pts',(-4.87291591474625,285.,-6.49381972833199));
#13265=CARTESIAN_POINT('Ctrl Pts',(-5.22082506112394,285.,-6.32959551460495));
#13266=CARTESIAN_POINT('Ctrl Pts',(-5.60001341231252,285.,-6.09157840023));
#13267=CARTESIAN_POINT('Ctrl Pts',(-6.53370549418297,285.,-5.26074061589865));
#13268=CARTESIAN_POINT('Ctrl Pts',(-7.06063989282633,285.000000000001,-4.64167227552575));
#13269=CARTESIAN_POINT('Ctrl Pts',(-7.81016526044142,285.000000000001,-3.30202932947539));
#13270=CARTESIAN_POINT('Ctrl Pts',(-8.05076497001306,284.999999999935,-2.7124664396346));
#13271=CARTESIAN_POINT('Ctrl Pts',(-8.40561382232048,284.999999999935,-1.41649823255915));
#13272=CARTESIAN_POINT('Ctrl Pts',(-8.5,285.,-0.709762093140782));
#13273=CARTESIAN_POINT('Ctrl Pts',(-8.5,285.,8.11850586757146E-14));
#13274=CARTESIAN_POINT('Origin',(-8.,318.,8.32667268468867E-14));
#13275=CARTESIAN_POINT('Origin',(-8.,317.501074056311,-0.0327551936970314));
#13276=CARTESIAN_POINT('Origin',(0.,285.,0.));
#13277=CARTESIAN_POINT('',(0.,0.,0.));
#13278=CARTESIAN_POINT('Origin',(0.,0.,-25.0375057290932));
#13279=CARTESIAN_POINT('',(-6.,-7.34788079488412E-16,-12.));
#13280=CARTESIAN_POINT('Origin',(0.,0.,-12.));
#13281=CARTESIAN_POINT('',(-6.,-7.34788079488412E-16,-11.9746));
#13282=CARTESIAN_POINT('',(-6.,-7.34788079488412E-16,-25.0375057290932));
#13283=CARTESIAN_POINT('',(6.,7.34788079488412E-16,-11.9746));
#13284=CARTESIAN_POINT('Origin',(0.,0.,-11.9746));
#13285=CARTESIAN_POINT('Origin',(0.,0.,-11.9746));
#13286=CARTESIAN_POINT('Origin',(0.,0.,-11.9746));
#13287=CARTESIAN_POINT('',(-5.1,6.2456986756515E-16,-11.3444132156113));
#13288=CARTESIAN_POINT('',(5.1,-6.2456986756515E-16,-11.3444132156113));
#13289=CARTESIAN_POINT('Origin',(0.,0.,-11.3444132156113));
#13290=CARTESIAN_POINT('',(6.,-7.34788079488412E-16,-11.9746));
#13291=CARTESIAN_POINT('Origin',(0.,0.,-11.3444132156113));
#13292=CARTESIAN_POINT('Origin',(0.,0.,-0.693205462827612));
#13293=CARTESIAN_POINT('',(-5.1,-6.2456986756515E-16,-0.63018678438874));
#13294=CARTESIAN_POINT('Origin',(0.,0.,-0.63018678438874));
#13295=CARTESIAN_POINT('',(-6.,-7.34788079488412E-16,8.32667268468867E-16));
#13296=CARTESIAN_POINT('',(-5.01,-6.13548046372824E-16,-0.693205462827612));
#13297=CARTESIAN_POINT('Origin',(0.,0.,0.));
#13298=CARTESIAN_POINT('Origin',(0.,0.,-10.2));
#13299=CARTESIAN_POINT('',(-12.389406481562,1.51726469909804E-15,-10.2));
#13300=CARTESIAN_POINT('',(12.389406481562,-1.51726469909804E-15,-10.2));
#13301=CARTESIAN_POINT('Origin',(0.,0.,-10.2));
#13302=CARTESIAN_POINT('',(9.47374549680553,1.47832800417317E-13,-9.13878618833741));
#13303=CARTESIAN_POINT('',(12.389406481562,-1.51726469909804E-15,-10.2));
#13304=CARTESIAN_POINT('',(9.50673733309445,-5.48871731080218,-9.68608426626664));
#13305=CARTESIAN_POINT('Ctrl Pts',(9.47374549680553,1.47832800417317E-13,
-9.13878618833741));
#13306=CARTESIAN_POINT('Ctrl Pts',(9.47374549680553,-0.917652977016494,
-9.1387861883374));
#13307=CARTESIAN_POINT('Ctrl Pts',(9.47742023919566,-1.84007744032089,-9.18998243378686));
#13308=CARTESIAN_POINT('Ctrl Pts',(9.48963681266947,-3.67190976040601,-9.38031285482134));
#13309=CARTESIAN_POINT('Ctrl Pts',(9.4979812322815,-4.58224166307851,-9.51835923202207));
#13310=CARTESIAN_POINT('Ctrl Pts',(9.50673734385392,-5.48871730453454,-9.6860842995786));
#13311=CARTESIAN_POINT('',(4.12011128382577E-8,-10.9774346929668,-9.68608426626665));
#13312=CARTESIAN_POINT('Ctrl Pts',(9.50673734443727,-5.48871736492593,-9.68608431075281));
#13313=CARTESIAN_POINT('Ctrl Pts',(8.71694238599845,-5.93459006657547,-9.51827723663476));
#13314=CARTESIAN_POINT('Ctrl Pts',(7.92188072226173,-6.38395964915516,-9.37991057108433));
#13315=CARTESIAN_POINT('Ctrl Pts',(6.33211805884209,-7.28773429047636,-9.19002022026341));
#13316=CARTESIAN_POINT('Ctrl Pts',(5.53677988505539,-7.74269267835578,-9.13897293541538));
#13317=CARTESIAN_POINT('Ctrl Pts',(3.94587469694457,-8.66117228117377,-9.13860048412926));
#13318=CARTESIAN_POINT('Ctrl Pts',(3.14812015320142,-9.12599280095263,-9.18970703534583));
#13319=CARTESIAN_POINT('Ctrl Pts',(1.56631645695501,-10.0533574210071,-9.3800550537477));
#13320=CARTESIAN_POINT('Ctrl Pts',(0.781382220745076,-10.5161833614735,
-9.51820254214856));
#13321=CARTESIAN_POINT('Ctrl Pts',(5.20087756022726E-8,-10.977434699151,
-9.68608429957861));
#13322=CARTESIAN_POINT('',(-9.5067372624267,-5.48871738635801,-9.68608422686381));
#13323=CARTESIAN_POINT('Ctrl Pts',(-8.03821811192016E-16,-10.9774347298519,
-9.68608431075282));
#13324=CARTESIAN_POINT('Ctrl Pts',(-0.781034565701908,-10.5163885828877,
-9.51827723663477));
#13325=CARTESIAN_POINT('Ctrl Pts',(-1.56773087177229,-10.0525297758065,
-9.37991057108433));
#13326=CARTESIAN_POINT('Ctrl Pts',(-3.14530400216244,-9.12764224395764,
-9.19002022026341));
#13327=CARTESIAN_POINT('Ctrl Pts',(-3.93697861062418,-8.66633837479854,
-9.13897293541538));
#13328=CARTESIAN_POINT('Ctrl Pts',(-5.52785787357781,-7.74781386829111,
-9.13860048412926));
#13329=CARTESIAN_POINT('Ctrl Pts',(-6.32928152377817,-7.28934842731451,
-9.18970703534583));
#13330=CARTESIAN_POINT('Ctrl Pts',(-7.92330469143949,-6.38314855259225,
-9.3800550537477));
#13331=CARTESIAN_POINT('Ctrl Pts',(-8.71659083151876,-5.9347885339675,-9.51820254214855));
#13332=CARTESIAN_POINT('Ctrl Pts',(-9.50673726236548,-5.48871741125893,
-9.68608429331509));
#13333=CARTESIAN_POINT('',(-9.47374541791149,5.30814753102003E-12,-9.13878640509698));
#13334=CARTESIAN_POINT('Ctrl Pts',(-9.5067372390073,-5.48871738714607,-9.68608418865576));
#13335=CARTESIAN_POINT('Ctrl Pts',(-9.50309533650332,-5.11181152183886,
-9.6163439615158));
#13336=CARTESIAN_POINT('Ctrl Pts',(-9.49952212465081,-4.73381646984127,
-9.5516635885274));
#13337=CARTESIAN_POINT('Ctrl Pts',(-9.49615224616066,-4.35510455307548,
-9.49309058903634));
#13338=CARTESIAN_POINT('Ctrl Pts',(-9.49313748707562,-4.01630147901212,
-9.44069004021243));
#13339=CARTESIAN_POINT('Ctrl Pts',(-9.49028561895122,-3.67692448753277,
-9.39317786501973));
#13340=CARTESIAN_POINT('Ctrl Pts',(-9.4876923009373,-3.33724242242393,-9.35126210844157));
#13341=CARTESIAN_POINT('Ctrl Pts',(-9.48625162146954,-3.1485370750109,-9.32797642980373));
#13342=CARTESIAN_POINT('Ctrl Pts',(-9.48489070945183,-2.95973763194223,
-9.30641711252709));
#13343=CARTESIAN_POINT('Ctrl Pts',(-9.48362561485523,-2.7708908093873,-9.28669845387052));
#13344=CARTESIAN_POINT('Ctrl Pts',(-9.4835827150424,-2.76448694570475,-9.28602978706251));
#13345=CARTESIAN_POINT('Ctrl Pts',(-9.48353993380462,-2.75808300240005,
-9.28536326917743));
#13346=CARTESIAN_POINT('Ctrl Pts',(-9.48349727158409,-2.75167898135504,
-9.28469890294303));
#13347=CARTESIAN_POINT('Ctrl Pts',(-9.48060306269765,-2.31722961643964,
-9.23962823771928));
#13348=CARTESIAN_POINT('Ctrl Pts',(-9.47825591393638,-1.88234724206654,
-9.20445631983736));
#13349=CARTESIAN_POINT('Ctrl Pts',(-9.47659088198413,-1.44699337073343,
-9.1799546918354));
#13350=CARTESIAN_POINT('Ctrl Pts',(-9.47498141340749,-1.02616758736896,
-9.15627070169182));
#13351=CARTESIAN_POINT('Ctrl Pts',(-9.47400932607905,-0.604901178862813,
-9.14255687393668));
#13352=CARTESIAN_POINT('Ctrl Pts',(-9.47379196605356,-0.183167756031004,
-9.13946164875121));
#13353=CARTESIAN_POINT('Ctrl Pts',(-9.47376050307898,-0.122121627911641,
-9.13901361332646));
#13354=CARTESIAN_POINT('Ctrl Pts',(-9.47374484508027,-0.0610657303984304,
-9.13878797893779));
#13355=CARTESIAN_POINT('Ctrl Pts',(-9.47374533901746,1.0764238021782E-11,
-9.13878662185656));
#13356=CARTESIAN_POINT('',(-9.50673733309446,5.48871731080218,-9.68608426626664));
#13357=CARTESIAN_POINT('Ctrl Pts',(-9.47374549680553,-1.47873570794491E-13,
-9.13878618833741));
#13358=CARTESIAN_POINT('Ctrl Pts',(-9.47374549680553,0.917652977016494,
-9.1387861883374));
#13359=CARTESIAN_POINT('Ctrl Pts',(-9.47742023919566,1.84007744032089,-9.18998243378686));
#13360=CARTESIAN_POINT('Ctrl Pts',(-9.48963681266947,3.67190976040601,-9.38031285482134));
#13361=CARTESIAN_POINT('Ctrl Pts',(-9.4979812322815,4.58224166307851,-9.51835923202207));
#13362=CARTESIAN_POINT('Ctrl Pts',(-9.50673734385392,5.48871730453454,-9.68608429957861));
#13363=CARTESIAN_POINT('',(-4.12011010549492E-8,10.9774346929669,-9.68608426626665));
#13364=CARTESIAN_POINT('Ctrl Pts',(-9.50673734443727,5.48871736492592,-9.68608431075281));
#13365=CARTESIAN_POINT('Ctrl Pts',(-8.71694238599846,5.93459006657546,-9.51827723663476));
#13366=CARTESIAN_POINT('Ctrl Pts',(-7.92188072226173,6.38395964915516,-9.37991057108432));
#13367=CARTESIAN_POINT('Ctrl Pts',(-6.33211805884209,7.28773429047635,-9.19002022026341));
#13368=CARTESIAN_POINT('Ctrl Pts',(-5.53677988505539,7.74269267835577,-9.13897293541538));
#13369=CARTESIAN_POINT('Ctrl Pts',(-3.94587469694457,8.66117228117376,-9.13860048412926));
#13370=CARTESIAN_POINT('Ctrl Pts',(-3.14812015320142,9.12599280095263,-9.18970703534583));
#13371=CARTESIAN_POINT('Ctrl Pts',(-1.56631645695502,10.0533574210071,-9.3800550537477));
#13372=CARTESIAN_POINT('Ctrl Pts',(-0.781382220745075,10.5161833614735,
-9.51820254214855));
#13373=CARTESIAN_POINT('Ctrl Pts',(-5.20087599329853E-8,10.977434699151,
-9.68608429957861));
#13374=CARTESIAN_POINT('',(9.50673729186498,5.48871738219012,-9.68608426617078));
#13375=CARTESIAN_POINT('Ctrl Pts',(3.04944243361098E-16,10.9774347298519,
-9.68608431075281));
#13376=CARTESIAN_POINT('Ctrl Pts',(0.781034565701908,10.5163885828877,-9.51827723663476));
#13377=CARTESIAN_POINT('Ctrl Pts',(1.56773087177229,10.0525297758065,-9.37991057108433));
#13378=CARTESIAN_POINT('Ctrl Pts',(3.14530400216244,9.12764224395764,-9.19002022026341));
#13379=CARTESIAN_POINT('Ctrl Pts',(3.93697861062418,8.66633837479853,-9.13897293541538));
#13380=CARTESIAN_POINT('Ctrl Pts',(5.52785787357781,7.7478138682911,-9.13860048412926));
#13381=CARTESIAN_POINT('Ctrl Pts',(6.32928152377817,7.2893484273145,-9.18970703534583));
#13382=CARTESIAN_POINT('Ctrl Pts',(7.92330469143948,6.38314855259225,-9.3800550537477));
#13383=CARTESIAN_POINT('Ctrl Pts',(8.71659083151876,5.93478853396749,-9.51820254214855));
#13384=CARTESIAN_POINT('Ctrl Pts',(9.50673729179886,5.48871739464254,-9.68608429956877));
#13385=CARTESIAN_POINT('Ctrl Pts',(9.50673734443727,5.48871736492592,-9.68608431075281));
#13386=CARTESIAN_POINT('Ctrl Pts',(9.49796877532218,4.58095205751653,-9.5181206164762));
#13387=CARTESIAN_POINT('Ctrl Pts',(9.48959593650276,3.66686690783038,-9.3796529749726));
#13388=CARTESIAN_POINT('Ctrl Pts',(9.47740359978457,1.836490901034,-9.18974634775445));
#13389=CARTESIAN_POINT('Ctrl Pts',(9.47374549680553,0.919367531929958,-9.13878618833741));
#13390=CARTESIAN_POINT('Ctrl Pts',(9.47374549680553,1.47832800417317E-13,
-9.13878618833741));
#13391=CARTESIAN_POINT('Origin',(0.,0.,-10.2));
#13392=CARTESIAN_POINT('Origin',(0.,0.,-11.0720179162868));
#13393=CARTESIAN_POINT('',(-12.0720179162868,-1.47839581004301E-15,-12.));
#13394=CARTESIAN_POINT('Origin',(-12.0720179162868,-1.47839581004302E-15,
-11.0720179162868));
#13395=CARTESIAN_POINT('Origin',(0.,0.,-12.));
#13396=CARTESIAN_POINT('Origin',(0.,0.,-12.));
#13397=CARTESIAN_POINT('',(-5.1,-6.2456986756515E-16,-12.));
#13398=CARTESIAN_POINT('Origin',(-2.35299013008461E-16,10.3923048454133,
-12.));
#13399=CARTESIAN_POINT('',(-2.35299013008461E-16,10.3923048454133,-8.93601699627353));
#13400=CARTESIAN_POINT('',(0.,10.3923048454133,-1.2));
#13401=CARTESIAN_POINT('',(-2.35299013008461E-16,10.3923048454133,-12.));
#13402=CARTESIAN_POINT('',(-9.00000000008138,5.19615066621323,-8.93601701787771));
#13403=CARTESIAN_POINT('Ctrl Pts',(-6.07852008438492E-6,10.3923013359781,
-8.93603703387842));
#13404=CARTESIAN_POINT('Ctrl Pts',(-0.301195462062673,10.2184095643127,
-8.87641996617827));
#13405=CARTESIAN_POINT('Ctrl Pts',(-0.602385138153431,10.0445176237446,
-8.82152809836376));
#13406=CARTESIAN_POINT('Ctrl Pts',(-0.903577682885929,9.87062402696534,
-8.77193268574838));
#13407=CARTESIAN_POINT('Ctrl Pts',(-1.19726885426351,9.70106135011187,-8.72357247537563));
#13408=CARTESIAN_POINT('Ctrl Pts',(-1.49096277600334,9.53149708533603,-8.6802482745101));
#13409=CARTESIAN_POINT('Ctrl Pts',(-1.78464966066903,9.36193688341683,-8.64244231384737));
#13410=CARTESIAN_POINT('Ctrl Pts',(-1.93979249065832,9.27236512875967,-8.62247096329028));
#13411=CARTESIAN_POINT('Ctrl Pts',(-2.09493314852878,9.1827946281759,-8.60403870988084));
#13412=CARTESIAN_POINT('Ctrl Pts',(-2.25006873511963,9.09322705549679,-8.58721096889182));
#13413=CARTESIAN_POINT('Ctrl Pts',(-2.57357704286633,8.90644944693415,-8.55211963923506));
#13414=CARTESIAN_POINT('Ctrl Pts',(-2.89698498406969,8.71972978502468,-8.52402127580572));
#13415=CARTESIAN_POINT('Ctrl Pts',(-3.22042421153454,8.53299206003282,-8.50343197405325));
#13416=CARTESIAN_POINT('Ctrl Pts',(-3.54650772650974,8.34472765493547,-8.48267434382096));
#13417=CARTESIAN_POINT('Ctrl Pts',(-3.87262302478416,8.15644489978108,-8.469549024806));
#13418=CARTESIAN_POINT('Ctrl Pts',(-4.19889273693572,7.96807299360913,-8.46453388744621));
#13419=CARTESIAN_POINT('Ctrl Pts',(-4.2877593691349,7.91676581957802,-8.46316790601863));
#13420=CARTESIAN_POINT('Ctrl Pts',(-4.37663738754378,7.86545207170697,-8.46240330115924));
#13421=CARTESIAN_POINT('Ctrl Pts',(-4.46552911497214,7.81413040892396,-8.46224908602198));
#13422=CARTESIAN_POINT('Ctrl Pts',(-4.47702295601336,7.80749443670175,-8.46222914576066));
#13423=CARTESIAN_POINT('Ctrl Pts',(-4.48851325102017,7.80086051178337,-8.46221928455636));
#13424=CARTESIAN_POINT('Ctrl Pts',(-4.50000000003849,7.79422863414232,-8.4622194678316));
#13425=CARTESIAN_POINT('Ctrl Pts',(-5.02158818205606,7.49308955670287,-8.46222778995974));
#13426=CARTESIAN_POINT('Ctrl Pts',(-5.5431711936851,7.19195346442769,-8.48297232998703));
#13427=CARTESIAN_POINT('Ctrl Pts',(-6.06475920079968,6.89081448843259,-8.52296987642172));
#13428=CARTESIAN_POINT('Ctrl Pts',(-6.29317060573264,6.75894110244808,-8.54048541675317));
#13429=CARTESIAN_POINT('Ctrl Pts',(-6.52158273068006,6.62706730087865,-8.56169255024703));
#13430=CARTESIAN_POINT('Ctrl Pts',(-6.74999529948836,6.49519324368519,-8.58646372999425));
#13431=CARTESIAN_POINT('Ctrl Pts',(-6.81977791240305,6.45490423360735,-8.59403160446263));
#13432=CARTESIAN_POINT('Ctrl Pts',(-6.88955873896841,6.4146162548414,-8.60193048700176));
#13433=CARTESIAN_POINT('Ctrl Pts',(-6.95933612940203,6.37433025985928,-8.61015656868989));
#13434=CARTESIAN_POINT('Ctrl Pts',(-7.30266835708907,6.17610730660974,-8.65063212866093));
#13435=CARTESIAN_POINT('Ctrl Pts',(-7.64602887829948,5.97786801610262,-8.69891514178612));
#13436=CARTESIAN_POINT('Ctrl Pts',(-7.98939420141902,5.77962595354147,-8.75415779946613));
#13437=CARTESIAN_POINT('Ctrl Pts',(-8.32626415664962,5.58513399339513,-8.80835544368486));
#13438=CARTESIAN_POINT('Ctrl Pts',(-8.66313875598589,5.3906393526244,-8.86925130743439));
#13439=CARTESIAN_POINT('Ctrl Pts',(-9.00000000000115,5.19615242270862,-8.93599629172134));
#13440=CARTESIAN_POINT('',(-9.,5.19615242270663,-1.2));
#13441=CARTESIAN_POINT('',(-9.,5.19615242270663,-12.));
#13442=CARTESIAN_POINT('',(-4.5,7.79422863405995,0.));
#13443=CARTESIAN_POINT('Ctrl Pts',(-8.99999999999999,5.19615242270665,-1.19999999999999));
#13444=CARTESIAN_POINT('Ctrl Pts',(-6.5884572681199,6.5884572681199,-3.99680288865056E-15));
#13445=CARTESIAN_POINT('Ctrl Pts',(-4.50000000000001,7.79422863405995,-3.78993143111475E-15));
#13446=CARTESIAN_POINT('Ctrl Pts',(-4.50000000000001,7.79422863405995,-3.78993143111475E-15));
#13447=CARTESIAN_POINT('Ctrl Pts',(-2.41154273188011,9.,-3.68820461000181E-15));
#13448=CARTESIAN_POINT('Ctrl Pts',(-1.63323345900868E-14,10.3923048454133,
-1.2));
#13449=CARTESIAN_POINT('Origin',(9.,5.19615242270663,-12.));
#13450=CARTESIAN_POINT('',(9.,5.19615242270663,-8.93601699627312));
#13451=CARTESIAN_POINT('',(9.,5.19615242270664,-1.2));
#13452=CARTESIAN_POINT('',(9.,5.19615242270663,-12.));
#13453=CARTESIAN_POINT('Ctrl Pts',(8.99999392148002,5.19615593214177,-8.93603703387764));
#13454=CARTESIAN_POINT('Ctrl Pts',(8.69880453793134,5.37004770381067,-8.87641996617583));
#13455=CARTESIAN_POINT('Ctrl Pts',(8.39761486183447,5.54393964438233,-8.82152809836008));
#13456=CARTESIAN_POINT('Ctrl Pts',(8.0964223170958,5.71783324116511,-8.77193268574382));
#13457=CARTESIAN_POINT('Ctrl Pts',(7.80273114570837,5.88739591802426,-8.72357247536959));
#13458=CARTESIAN_POINT('Ctrl Pts',(7.50903722395865,6.05696018280582,-8.68024827450306));
#13459=CARTESIAN_POINT('Ctrl Pts',(7.21535033928308,6.22652038473072,-8.6424423138398));
#13460=CARTESIAN_POINT('Ctrl Pts',(7.06020750930979,6.31609213937864,-8.62247096328515));
#13461=CARTESIAN_POINT('Ctrl Pts',(6.90506685145532,6.40566263995317,-8.60403870987786));
#13462=CARTESIAN_POINT('Ctrl Pts',(6.74993126488047,6.49523021262305,-8.58721096889069));
#13463=CARTESIAN_POINT('Ctrl Pts',(6.42642295713265,6.68200782118634,-8.55211963923401));
#13464=CARTESIAN_POINT('Ctrl Pts',(6.10301501593021,6.86872748309998,-8.52402127580485));
#13465=CARTESIAN_POINT('Ctrl Pts',(5.77957578850881,7.05546520816967,-8.50343197405257));
#13466=CARTESIAN_POINT('Ctrl Pts',(5.45349227355191,7.24372961336021,-8.48267434381885));
#13467=CARTESIAN_POINT('Ctrl Pts',(5.12737697532985,7.43201236866678,-8.46954902480367));
#13468=CARTESIAN_POINT('Ctrl Pts',(4.80110726312322,7.62038427480488,-8.46453388744491));
#13469=CARTESIAN_POINT('Ctrl Pts',(4.712240630944,7.67169144880659,-8.46316790601815));
#13470=CARTESIAN_POINT('Ctrl Pts',(4.62336261254755,7.72300519663518,-8.46240330115919));
#13471=CARTESIAN_POINT('Ctrl Pts',(4.53447088512655,7.7743268593669,-8.46224908602198));
#13472=CARTESIAN_POINT('Ctrl Pts',(4.5229770440827,7.78096283158455,-8.46222914576066));
#13473=CARTESIAN_POINT('Ctrl Pts',(4.51148674907318,7.78759675649823,-8.46221928455636));
#13474=CARTESIAN_POINT('Ctrl Pts',(4.5000000000521,7.79422863413447,-8.4622194678316));
#13475=CARTESIAN_POINT('Ctrl Pts',(3.97841181773793,8.0953677114542,-8.46222778995974));
#13476=CARTESIAN_POINT('Ctrl Pts',(3.45682880584612,8.39650380366825,-8.48297233000062));
#13477=CARTESIAN_POINT('Ctrl Pts',(2.93524079883684,8.69764278023972,-8.52296987646097));
#13478=CARTESIAN_POINT('Ctrl Pts',(2.70682939419531,8.829516166335,-8.54048541678485));
#13479=CARTESIAN_POINT('Ctrl Pts',(2.47841726963945,8.96138996818865,-8.56169255026554));
#13480=CARTESIAN_POINT('Ctrl Pts',(2.25000470177625,9.09326402662507,-8.58646372999426));
#13481=CARTESIAN_POINT('Ctrl Pts',(2.18022208909817,9.13355303711273,-8.59403160446263));
#13482=CARTESIAN_POINT('Ctrl Pts',(2.11044126273703,9.17384101623243,-8.60193048700176));
#13483=CARTESIAN_POINT('Ctrl Pts',(2.04066387244898,9.21412701146667,-8.61015656868988));
#13484=CARTESIAN_POINT('Ctrl Pts',(1.69733164548179,9.4123499659547,-8.65063212866048));
#13485=CARTESIAN_POINT('Ctrl Pts',(1.35397112327281,9.61058925472395,-8.69891514178508));
#13486=CARTESIAN_POINT('Ctrl Pts',(1.01060579944003,9.80883131604148,-8.75415779946437));
#13487=CARTESIAN_POINT('Ctrl Pts',(0.673735843502585,10.0033232749718,-8.80835544368355));
#13488=CARTESIAN_POINT('Ctrl Pts',(0.33686124402347,10.1978179155034,-8.86925130743368));
#13489=CARTESIAN_POINT('Ctrl Pts',(1.15152427354714E-12,10.3923048454153,
-8.93599629172134));
#13490=CARTESIAN_POINT('',(4.5,7.79422863405995,0.));
#13491=CARTESIAN_POINT('Ctrl Pts',(1.4874090430258E-14,10.3923048454133,
-1.19999999999999));
#13492=CARTESIAN_POINT('Ctrl Pts',(2.41154273188011,9.,2.99760216648792E-15));
#13493=CARTESIAN_POINT('Ctrl Pts',(4.50000000000001,7.79422863405994,2.1656751034942E-15));
#13494=CARTESIAN_POINT('Ctrl Pts',(4.50000000000001,7.79422863405994,2.1656751034942E-15));
#13495=CARTESIAN_POINT('Ctrl Pts',(6.58845726811989,6.5884572681199,1.23696196253983E-15));
#13496=CARTESIAN_POINT('Ctrl Pts',(8.99999999999997,5.19615242270665,-1.19999999999998));
#13497=CARTESIAN_POINT('Origin',(9.,5.19615242270663,-12.));
#13498=CARTESIAN_POINT('',(9.,-5.19615242270664,-8.93601701652031));
#13499=CARTESIAN_POINT('',(9.,-5.19615242270664,-1.2));
#13500=CARTESIAN_POINT('',(9.,-5.19615242270664,-12.));
#13501=CARTESIAN_POINT('Ctrl Pts',(9.,-5.19614539697823,-8.93603707371988));
#13502=CARTESIAN_POINT('Ctrl Pts',(9.,-4.84829207744338,-8.87640809817269));
#13503=CARTESIAN_POINT('Ctrl Pts',(9.,-4.5004384103798,-8.82150625311342));
#13504=CARTESIAN_POINT('Ctrl Pts',(9.,-4.15258143955633,-8.77190307482733));
#13505=CARTESIAN_POINT('Ctrl Pts',(9.,-3.81338948504499,-8.72353549733419));
#13506=CARTESIAN_POINT('Ctrl Pts',(9.,-3.47419436295703,-8.68020598944004));
#13507=CARTESIAN_POINT('Ctrl Pts',(9.,-3.13500738320275,-8.64239703270597));
#13508=CARTESIAN_POINT('Ctrl Pts',(9.,-2.95600024043739,-8.62244322044345));
#13509=CARTESIAN_POINT('Ctrl Pts',(9.,-2.77699560569171,-8.60402620280014));
#13510=CARTESIAN_POINT('Ctrl Pts',(9.,-2.59799681666225,-8.58721124573255));
#13511=CARTESIAN_POINT('Ctrl Pts',(9.,-2.22450410506814,-8.55212573512904));
#13512=CARTESIAN_POINT('Ctrl Pts',(9.00000000000212,-1.85112676034851,-8.52403085874111));
#13513=CARTESIAN_POINT('Ctrl Pts',(9.0000000000486,-1.47771346656234,-8.50344248169531));
#13514=CARTESIAN_POINT('Ctrl Pts',(9.00000000009545,-1.10129661789082,-8.48268850175993));
#13515=CARTESIAN_POINT('Ctrl Pts',(9.00000000017784,-0.724843258692337,
-8.46956223116017));
#13516=CARTESIAN_POINT('Ctrl Pts',(9.00000000014829,-0.348212540979102,
-8.46454110270077));
#13517=CARTESIAN_POINT('Ctrl Pts',(9.00000000014023,-0.245516126139824,
-8.46317198471072));
#13518=CARTESIAN_POINT('Ctrl Pts',(9.0000000001243,-0.142806604662479,-8.46240519271688));
#13519=CARTESIAN_POINT('Ctrl Pts',(9.00000000010304,-0.0400813005700133,
-8.46224976049714));
#13520=CARTESIAN_POINT('Ctrl Pts',(9.00000000010027,-0.0267167643637567,
-8.46222953880448));
#13521=CARTESIAN_POINT('Ctrl Pts',(9.00000000009742,-0.0133563304832161,
-8.46221953990594));
#13522=CARTESIAN_POINT('Ctrl Pts',(9.00000000009451,-8.15016804301746E-12,
-8.46221972848024));
#13523=CARTESIAN_POINT('Ctrl Pts',(8.99999999995155,0.654989413214678,-8.46222897609269));
#13524=CARTESIAN_POINT('Ctrl Pts',(8.99999999976969,1.30997129101454,-8.48676659793625));
#13525=CARTESIAN_POINT('Ctrl Pts',(9.00000000024692,1.96496169710869,-8.53391508241261));
#13526=CARTESIAN_POINT('Ctrl Pts',(9.00000000040068,2.17599761070563,-8.54910618048611));
#13527=CARTESIAN_POINT('Ctrl Pts',(9.0000000006655,2.3870340834294,-8.56664433473375));
#13528=CARTESIAN_POINT('Ctrl Pts',(9.00000000130499,2.59807069766354,-8.58646463712839));
#13529=CARTESIAN_POINT('Ctrl Pts',(9.00000000154905,2.67861189655562,-8.59402896866896));
#13530=CARTESIAN_POINT('Ctrl Pts',(9.00000000175971,2.75915062264558,-8.60192400520041));
#13531=CARTESIAN_POINT('Ctrl Pts',(9.00000000190986,2.83968469038153,-8.61014594910981));
#13532=CARTESIAN_POINT('Ctrl Pts',(9.0000000026465,3.23477341913773,-8.65048164130054));
#13533=CARTESIAN_POINT('Ctrl Pts',(9.0000000016216,3.62990043667534,-8.6985717486516));
#13534=CARTESIAN_POINT('Ctrl Pts',(9.00000000088224,4.02503435673907,-8.75357741709708));
#13535=CARTESIAN_POINT('Ctrl Pts',(9.00000000015179,4.41540872345877,-8.80792051925833));
#13536=CARTESIAN_POINT('Ctrl Pts',(9.00000000000588,4.80578984875463,-8.86901301455119));
#13537=CARTESIAN_POINT('Ctrl Pts',(9.00000000000233,5.19615242270663,-8.93599629172134));
#13538=CARTESIAN_POINT('',(9.,0.,0.));
#13539=CARTESIAN_POINT('Ctrl Pts',(9.,0.,1.62425632676704E-15));
#13540=CARTESIAN_POINT('Ctrl Pts',(9.,2.4115427318801,1.49904191230263E-15));
#13541=CARTESIAN_POINT('Ctrl Pts',(9.,5.19615242270662,-1.19999999999999));
#13542=CARTESIAN_POINT('Ctrl Pts',(9.,-5.19615242270662,-1.19999999999999));
#13543=CARTESIAN_POINT('Ctrl Pts',(9.,-2.4115427318801,1.33226762955019E-15));
#13544=CARTESIAN_POINT('Ctrl Pts',(9.,0.,1.62425632676704E-15));
#13545=CARTESIAN_POINT('Origin',(0.,-10.3923048454133,-12.));
#13546=CARTESIAN_POINT('',(0.,-10.3923048454133,-8.93601699627358));
#13547=CARTESIAN_POINT('',(-1.30104260698261E-14,-10.3923048454133,-1.2));
#13548=CARTESIAN_POINT('',(0.,-10.3923048454133,-12.));
#13549=CARTESIAN_POINT('Ctrl Pts',(6.07852010015009E-6,-10.3923013359781,
-8.93603703387852));
#13550=CARTESIAN_POINT('Ctrl Pts',(0.30119546205775,-10.2184095643155,-8.87641996617938));
#13551=CARTESIAN_POINT('Ctrl Pts',(0.602385138143551,-10.0445176237503,
-8.82152809836565));
#13552=CARTESIAN_POINT('Ctrl Pts',(0.903577682871094,-9.87062402697391,
-8.77193268575082));
#13553=CARTESIAN_POINT('Ctrl Pts',(1.1972688542489,-9.70106135012032,-8.72357247537779));
#13554=CARTESIAN_POINT('Ctrl Pts',(1.49096277598897,-9.53149708534433,-8.68024827451193));
#13555=CARTESIAN_POINT('Ctrl Pts',(1.78464966065489,-9.361936883425,-8.64244231384889));
#13556=CARTESIAN_POINT('Ctrl Pts',(1.93979249064888,-9.27236512876513,-8.62247096329104));
#13557=CARTESIAN_POINT('Ctrl Pts',(2.09493314852404,-9.18279462817865,-8.60403870988093));
#13558=CARTESIAN_POINT('Ctrl Pts',(2.25006873511959,-9.09322705549682,-8.58721096889136));
#13559=CARTESIAN_POINT('Ctrl Pts',(2.57357704286724,-8.90644944693363,-8.55211963923438));
#13560=CARTESIAN_POINT('Ctrl Pts',(2.89698498407157,-8.7197297850236,-8.52402127580505));
#13561=CARTESIAN_POINT('Ctrl Pts',(3.22042421153739,-8.53299206003118,-8.5034319740527));
#13562=CARTESIAN_POINT('Ctrl Pts',(3.54650772651119,-8.34472765493464,-8.48267434382068));
#13563=CARTESIAN_POINT('Ctrl Pts',(3.87262302478421,-8.15644489978106,-8.46954902480601));
#13564=CARTESIAN_POINT('Ctrl Pts',(4.19889273693436,-7.96807299360993,-8.46453388744643));
#13565=CARTESIAN_POINT('Ctrl Pts',(4.28775936913399,-7.91676581957855,-8.46316790601889));
#13566=CARTESIAN_POINT('Ctrl Pts',(4.37663738754333,-7.86545207170724,-8.46240330115955));
#13567=CARTESIAN_POINT('Ctrl Pts',(4.46552911497214,-7.81413040892397,-8.46224908602234));
#13568=CARTESIAN_POINT('Ctrl Pts',(4.47702295601336,-7.80749443670175,-8.46222914576103));
#13569=CARTESIAN_POINT('Ctrl Pts',(4.48851325102017,-7.80086051178337,-8.46221928455673));
#13570=CARTESIAN_POINT('Ctrl Pts',(4.50000000003849,-7.79422863414233,-8.46221946783198));
#13571=CARTESIAN_POINT('Ctrl Pts',(5.02158818224417,-7.49308955659427,-8.46222778996038));
#13572=CARTESIAN_POINT('Ctrl Pts',(5.54317119406134,-7.19195346421047,-8.48297233000241));
#13573=CARTESIAN_POINT('Ctrl Pts',(6.06475920136405,-6.89081448810676,-8.52296987646522));
#13574=CARTESIAN_POINT('Ctrl Pts',(6.29317060610888,-6.75894110223086,-8.54048541678825));
#13575=CARTESIAN_POINT('Ctrl Pts',(6.52158273086818,-6.62706730077005,-8.56169255026751));
#13576=CARTESIAN_POINT('Ctrl Pts',(6.74999529948835,-6.4951932436852,-8.58646372999432));
#13577=CARTESIAN_POINT('Ctrl Pts',(6.81977791240305,-6.45490423360736,-8.59403160446269));
#13578=CARTESIAN_POINT('Ctrl Pts',(6.88955873896841,-6.4146162548414,-8.60193048700183));
#13579=CARTESIAN_POINT('Ctrl Pts',(6.95933612940203,-6.37433025985929,-8.61015656868998));
#13580=CARTESIAN_POINT('Ctrl Pts',(7.30266835710366,-6.17610730660132,-8.65063212866286));
#13581=CARTESIAN_POINT('Ctrl Pts',(7.64602887832874,-5.97786801608574,-8.69891514179043));
#13582=CARTESIAN_POINT('Ctrl Pts',(7.98939420146296,-5.77962595351611,-8.75415779947333));
#13583=CARTESIAN_POINT('Ctrl Pts',(8.32626415667892,-5.58513399337823,-8.80835544369024));
#13584=CARTESIAN_POINT('Ctrl Pts',(8.66313875600055,-5.39063935261595,-8.8692513074373));
#13585=CARTESIAN_POINT('Ctrl Pts',(9.00000000000115,-5.19615242270863,-8.93599629172134));
#13586=CARTESIAN_POINT('',(4.5,-7.79422863405995,0.));
#13587=CARTESIAN_POINT('Ctrl Pts',(8.99999999999998,-5.19615242270664,-1.19999999999999));
#13588=CARTESIAN_POINT('Ctrl Pts',(6.58845726811989,-6.5884572681199,-2.44249065417534E-15));
#13589=CARTESIAN_POINT('Ctrl Pts',(4.5,-7.79422863405995,-2.97780326730443E-15));
#13590=CARTESIAN_POINT('Ctrl Pts',(4.5,-7.79422863405995,-2.97780326730443E-15));
#13591=CARTESIAN_POINT('Ctrl Pts',(2.41154273188012,-9.,-3.41478402099401E-15));
#13592=CARTESIAN_POINT('Ctrl Pts',(2.42068530531642E-14,-10.3923048454133,
-1.19999999999999));
#13593=CARTESIAN_POINT('Origin',(-9.,-5.19615242270664,-12.));
#13594=CARTESIAN_POINT('',(-9.,-5.19615242270664,-8.93601699627313));
#13595=CARTESIAN_POINT('',(-9.,-5.19615242270664,-1.2));
#13596=CARTESIAN_POINT('',(-9.,-5.19615242270664,-12.));
#13597=CARTESIAN_POINT('Ctrl Pts',(-8.99999392148003,-5.19615593214178,
-8.93603703387762));
#13598=CARTESIAN_POINT('Ctrl Pts',(-8.69880453793641,-5.37004770380774,
-8.87641996617677));
#13599=CARTESIAN_POINT('Ctrl Pts',(-8.3976148618446,-5.54393964437648,-8.82152809836176));
#13600=CARTESIAN_POINT('Ctrl Pts',(-8.09642231711102,-5.71783324115633,
-8.77193268574606));
#13601=CARTESIAN_POINT('Ctrl Pts',(-7.80273114573057,-5.88739591801145,
-8.72357247537269));
#13602=CARTESIAN_POINT('Ctrl Pts',(-7.50903722398783,-6.05696018278898,
-8.68024827450678));
#13603=CARTESIAN_POINT('Ctrl Pts',(-7.21535033931923,-6.22652038470985,
-8.64244231384387));
#13604=CARTESIAN_POINT('Ctrl Pts',(-7.06020750933391,-6.31609213936472,
-8.62247096328738));
#13605=CARTESIAN_POINT('Ctrl Pts',(-6.90506685146741,-6.4056626399462,-8.6040387098785));
#13606=CARTESIAN_POINT('Ctrl Pts',(-6.74993126488053,-6.49523021262302,
-8.58721096888999));
#13607=CARTESIAN_POINT('Ctrl Pts',(-6.4264229571074,-6.68200782120092,-8.5521196392305));
#13608=CARTESIAN_POINT('Ctrl Pts',(-6.10301501587966,-6.86872748312918,
-8.5240212757998));
#13609=CARTESIAN_POINT('Ctrl Pts',(-5.77957578843295,-7.05546520821348,
-8.50343197404727));
#13610=CARTESIAN_POINT('Ctrl Pts',(-5.45349227348263,-7.24372961340022,
-8.48267434381534));
#13611=CARTESIAN_POINT('Ctrl Pts',(-5.12737697526716,-7.43201236870298,
-8.46954902480175));
#13612=CARTESIAN_POINT('Ctrl Pts',(-4.80110726306711,-7.62038427483728,
-8.46453388744425));
#13613=CARTESIAN_POINT('Ctrl Pts',(-4.71224063090659,-7.67169144882819,
-8.46316790601809));
#13614=CARTESIAN_POINT('Ctrl Pts',(-4.62336261252885,-7.72300519664598,
-8.46240330115948));
#13615=CARTESIAN_POINT('Ctrl Pts',(-4.53447088512656,-7.7743268593669,-8.46224908602235));
#13616=CARTESIAN_POINT('Ctrl Pts',(-4.5229770440827,-7.78096283158455,-8.46222914576104));
#13617=CARTESIAN_POINT('Ctrl Pts',(-4.51148674907318,-7.78759675649824,
-8.46221928455675));
#13618=CARTESIAN_POINT('Ctrl Pts',(-4.50000000005209,-7.79422863413447,
-8.46221946783199));
#13619=CARTESIAN_POINT('Ctrl Pts',(-3.97841181786548,-8.09536771138056,
-8.46222778996039));
#13620=CARTESIAN_POINT('Ctrl Pts',(-3.45682880610124,-8.39650380352096,
-8.48297232999122));
#13621=CARTESIAN_POINT('Ctrl Pts',(-2.9352407992195,-8.69764278001881,-8.52296987643228));
#13622=CARTESIAN_POINT('Ctrl Pts',(-2.70682939445042,-8.82951616618772,
-8.54048541676178));
#13623=CARTESIAN_POINT('Ctrl Pts',(-2.47841726976704,-8.961389968115,-8.56169255025224));
#13624=CARTESIAN_POINT('Ctrl Pts',(-2.25000470177628,-9.09326402662505,
-8.58646372999467));
#13625=CARTESIAN_POINT('Ctrl Pts',(-2.1802220890982,-9.13355303711272,-8.59403160446301));
#13626=CARTESIAN_POINT('Ctrl Pts',(-2.11044126273707,-9.17384101623242,
-8.6019304870021));
#13627=CARTESIAN_POINT('Ctrl Pts',(-2.04066387244902,-9.21412701146666,
-8.61015656869019));
#13628=CARTESIAN_POINT('Ctrl Pts',(-1.69733164547995,-9.41234996595577,
-8.65063212866084));
#13629=CARTESIAN_POINT('Ctrl Pts',(-1.35397112326908,-9.61058925472611,
-8.69891514178567));
#13630=CARTESIAN_POINT('Ctrl Pts',(-1.01060579943443,-9.80883131604472,
-8.75415779946531));
#13631=CARTESIAN_POINT('Ctrl Pts',(-0.67373584349885,-10.003323274974,-8.80835544368422));
#13632=CARTESIAN_POINT('Ctrl Pts',(-0.336861244021614,-10.1978179155045,
-8.86925130743406));
#13633=CARTESIAN_POINT('Ctrl Pts',(-1.15285654227901E-12,-10.3923048454153,
-8.93599629172134));
#13634=CARTESIAN_POINT('',(-4.5,-7.79422863405995,0.));
#13635=CARTESIAN_POINT('Ctrl Pts',(-2.36235553892334E-14,-10.3923048454133,
-1.19999999999999));
#13636=CARTESIAN_POINT('Ctrl Pts',(-2.41154273188012,-9.,-1.33226762955019E-15));
#13637=CARTESIAN_POINT('Ctrl Pts',(-4.5,-7.79422863405995,-1.0828375517471E-15));
#13638=CARTESIAN_POINT('Ctrl Pts',(-4.5,-7.79422863405995,-1.0828375517471E-15));
#13639=CARTESIAN_POINT('Ctrl Pts',(-6.58845726811989,-6.58845726811991,
-1.18980142210385E-15));
#13640=CARTESIAN_POINT('Ctrl Pts',(-8.99999999999998,-5.19615242270665,
-1.19999999999999));
#13641=CARTESIAN_POINT('Origin',(-9.,5.19615242270663,-12.));
#13642=CARTESIAN_POINT('Ctrl Pts',(-9.,5.19614539650958,-8.93603707639091));
#13643=CARTESIAN_POINT('Ctrl Pts',(-9.,4.84832857664298,-8.87641436251837));
#13644=CARTESIAN_POINT('Ctrl Pts',(-9.,4.50051141122661,-8.82151779810304));
#13645=CARTESIAN_POINT('Ctrl Pts',(-9.,4.15269093788426,-8.77191875049037));
#13646=CARTESIAN_POINT('Ctrl Pts',(-9.,3.81353345495309,-8.72355504152739));
#13647=CARTESIAN_POINT('Ctrl Pts',(-9.,3.47437280046155,-8.68022834191494));
#13648=CARTESIAN_POINT('Ctrl Pts',(-9.,3.13522028344948,-8.64242098329983));
#13649=CARTESIAN_POINT('Ctrl Pts',(-9.,2.9561421598243,-8.62245807428277));
#13650=CARTESIAN_POINT('Ctrl Pts',(-9.,2.7770665453474,-8.60403315443626));
#13651=CARTESIAN_POINT('Ctrl Pts',(-9.,2.59799678343793,-8.58721156446757));
#13652=CARTESIAN_POINT('Ctrl Pts',(-9.,2.22433287352971,-8.55211004307419));
#13653=CARTESIAN_POINT('Ctrl Pts',(-9.00000000000195,1.85078513355755,-8.52400542530791));
#13654=CARTESIAN_POINT('Ctrl Pts',(-9.00000000004448,1.4772011518465,-8.50341433154624));
#13655=CARTESIAN_POINT('Ctrl Pts',(-9.00000000008736,1.10053656913797,-8.48265344211055));
#13656=CARTESIAN_POINT('Ctrl Pts',(-9.00000000016269,0.723835163596231,
-8.46953046790419));
#13657=CARTESIAN_POINT('Ctrl Pts',(-9.00000000013545,0.346954913253201,
-8.46452392492529));
#13658=CARTESIAN_POINT('Ctrl Pts',(-9.00000000012805,0.244465457900586,
-8.46316243712475));
#13659=CARTESIAN_POINT('Ctrl Pts',(-9.00000000011348,0.141962856303526,
-8.46240089073438));
#13660=CARTESIAN_POINT('Ctrl Pts',(-9.00000000009406,0.0394444306228228,
-8.46224826955939));
#13661=CARTESIAN_POINT('Ctrl Pts',(-9.00000000009157,0.0262922197916786,
-8.46222868960723));
#13662=CARTESIAN_POINT('Ctrl Pts',(-9.00000000008901,0.013144076632877,
-8.46221900508837));
#13663=CARTESIAN_POINT('Ctrl Pts',(-9.00000000008638,7.53135263285704E-12,
-8.46221918237743));
#13664=CARTESIAN_POINT('Ctrl Pts',(-8.99999999997667,-0.549916859676629,
-8.46222659972942));
#13665=CARTESIAN_POINT('Ctrl Pts',(-8.99999999993513,-1.09982934347759,
-8.47951821623097));
#13666=CARTESIAN_POINT('Ctrl Pts',(-9.00000000008774,-1.64974515680917,
-8.51297261954941));
#13667=CARTESIAN_POINT('Ctrl Pts',(-9.00000000017546,-1.96585272030167,
-8.53220318114577));
#13668=CARTESIAN_POINT('Ctrl Pts',(-9.00000000032562,-2.28196122532694,
-8.5567735078678));
#13669=CARTESIAN_POINT('Ctrl Pts',(-9.0000000012242,-2.5980708693782,-8.58646281049615));
#13670=CARTESIAN_POINT('Ctrl Pts',(-9.0000000014534,-2.67869870244963,-8.59403544923519));
#13671=CARTESIAN_POINT('Ctrl Pts',(-9.00000000165122,-2.75932489265377,
-8.60193950572842));
#13672=CARTESIAN_POINT('Ctrl Pts',(-9.0000000017922,-2.83994782092948,-8.61017115770036));
#13673=CARTESIAN_POINT('Ctrl Pts',(-9.00000000248791,-3.23780289414195,
-8.65079241232356));
#13674=CARTESIAN_POINT('Ctrl Pts',(-9.00000000150868,-3.63568481736304,
-8.69927635641474));
#13675=CARTESIAN_POINT('Ctrl Pts',(-9.00000000081449,-4.03357090898489,
-8.75476582106047));
#13676=CARTESIAN_POINT('Ctrl Pts',(-9.00000000013838,-4.42109951253233,
-8.80881082338287));
#13677=CARTESIAN_POINT('Ctrl Pts',(-9.00000000000569,-4.80863209974855,
-8.86950072341166));
#13678=CARTESIAN_POINT('Ctrl Pts',(-9.00000000000228,-5.19615242270664,
-8.93599629172134));
#13679=CARTESIAN_POINT('',(-9.,0.,0.));
#13680=CARTESIAN_POINT('Ctrl Pts',(-9.,-5.19615242270662,-1.19999999999999));
#13681=CARTESIAN_POINT('Ctrl Pts',(-9.,-2.4115427318801,3.66373598126302E-15));
#13682=CARTESIAN_POINT('Ctrl Pts',(-9.,1.08283755047889E-14,1.62425632571833E-15));
#13683=CARTESIAN_POINT('Ctrl Pts',(-9.,1.08283755047889E-14,1.62425632571833E-15));
#13684=CARTESIAN_POINT('Ctrl Pts',(-9.,2.41154273188011,-7.86239849479496E-16));
#13685=CARTESIAN_POINT('Ctrl Pts',(-9.,5.19615242270663,-1.2));
#13686=CARTESIAN_POINT('Origin',(-18.,-3.46944695195361E-15,0.));
#13687=CARTESIAN_POINT('Origin',(0.,0.,0.));
#13688=CARTESIAN_POINT('Origin',(0.,0.,0.));
#13689=CARTESIAN_POINT('Origin',(0.,0.,0.));
#13690=CARTESIAN_POINT('Origin',(0.,0.,0.));
#13691=CARTESIAN_POINT('Origin',(0.,0.,0.));
#13692=CARTESIAN_POINT('Origin',(0.,0.,0.));
#13693=CARTESIAN_POINT('Origin',(-18.,-3.46944695195361E-15,-12.));
#13694=CARTESIAN_POINT('Origin',(0.,0.,0.));
#13695=CARTESIAN_POINT('Origin',(0.,0.,0.));
#13696=CARTESIAN_POINT('Origin',(0.,0.,0.));
#13697=CARTESIAN_POINT('Origin',(0.,0.,0.));
#13698=CARTESIAN_POINT('Origin',(0.,0.,0.));
#13699=CARTESIAN_POINT('Origin',(0.,0.,0.));
#13700=CARTESIAN_POINT('Ctrl Pts',(-9.41651585048208,-4.95567688430906,
-9.02143340818646));
#13701=CARTESIAN_POINT('Ctrl Pts',(-9.33347922663126,-5.00361810144193,
-9.54376732265014));
#13702=CARTESIAN_POINT('Ctrl Pts',(-9.56264608596435,-5.45717682649977,
-9.69801774536269));
#13703=CARTESIAN_POINT('Ctrl Pts',(-7.82828519779296,-5.87264227917434,
-8.68478716584893));
#13704=CARTESIAN_POINT('Ctrl Pts',(-7.78096540982093,-5.89996237149985,
-9.20046647829273));
#13705=CARTESIAN_POINT('Ctrl Pts',(-7.99064761656677,-6.34458248438458,
-9.36117071967683));
#13706=CARTESIAN_POINT('Ctrl Pts',(-6.20942222566736,-6.80729325191217,
-8.46511979781123));
#13707=CARTESIAN_POINT('Ctrl Pts',(-6.17732188361541,-6.82582639303532,
-8.96938931321266));
#13708=CARTESIAN_POINT('Ctrl Pts',(-6.40309790806795,-7.24276319894628,
-9.14170490909588));
#13709=CARTESIAN_POINT('Ctrl Pts',(-3.69699523786471,-8.25784364963932,
-8.4607958473145));
#13710=CARTESIAN_POINT('Ctrl Pts',(-3.7121972466429,-8.24906676577982,-8.96490808900259));
#13711=CARTESIAN_POINT('Ctrl Pts',(-3.95417133760969,-8.65630407204171,
-9.13738096492018));
#13712=CARTESIAN_POINT('Ctrl Pts',(-2.86553968521064,-8.73788473678336,
-8.51288388844084));
#13713=CARTESIAN_POINT('Ctrl Pts',(-2.89372401459971,-8.72161250662362,
-9.01926238740844));
#13714=CARTESIAN_POINT('Ctrl Pts',(-3.14556979243607,-9.12747462876032,
-9.18946890902302));
#13715=CARTESIAN_POINT('Ctrl Pts',(-1.21577897758477,-9.69037452542962,
-8.70732652632404));
#13716=CARTESIAN_POINT('Ctrl Pts',(-1.27236213191392,-9.65770622604611,
-9.22034895088592));
#13717=CARTESIAN_POINT('Ctrl Pts',(-1.53900867015813,-10.0694227766623,
-9.38391126097275));
#13718=CARTESIAN_POINT('Ctrl Pts',(-0.396828014250257,-10.1631960845639,
-8.84899630416932));
#13719=CARTESIAN_POINT('Ctrl Pts',(-0.465016578930744,-10.1238273983887,
-9.36716113818611));
#13720=CARTESIAN_POINT('Ctrl Pts',(-0.74038577260122,-10.5403775350051,
-9.5255700245206));
#13721=CARTESIAN_POINT('Ctrl Pts',(0.417977369734739,-10.6336241923448,
-9.02174323061994));
#13722=CARTESIAN_POINT('Ctrl Pts',(0.334920910614397,-10.5856715233137,
-9.54408615058461));
#13723=CARTESIAN_POINT('Ctrl Pts',(0.0566989198404312,-11.0109268220334,
-9.6983275674176));
#13724=CARTESIAN_POINT('Ctrl Pts',(-9.5067372390073,-5.48871738714607,-9.68608418865576));
#13725=CARTESIAN_POINT('Ctrl Pts',(-9.4675108481587,-5.46606999446181,-9.66959818350506));
#13726=CARTESIAN_POINT('Ctrl Pts',(-9.42925913707253,-5.4439810970595,-9.64980240749262));
#13727=CARTESIAN_POINT('Ctrl Pts',(-9.39245990190791,-5.42272474549804,
-9.62687223341926));
#13728=CARTESIAN_POINT('Ctrl Pts',(-9.35128004286391,-5.3989380130517,-9.60121242467673));
#13729=CARTESIAN_POINT('Ctrl Pts',(-9.31191221316965,-5.37619344504106,
-9.57162843008722));
#13730=CARTESIAN_POINT('Ctrl Pts',(-9.2749983072906,-5.35488193328893,-9.5383540974491));
#13731=CARTESIAN_POINT('Ctrl Pts',(-9.248186554751,-5.33940269949517,-9.51418588356417));
#13732=CARTESIAN_POINT('Ctrl Pts',(-9.22266843593477,-5.32467985874466,
-9.48806920949896));
#13733=CARTESIAN_POINT('Ctrl Pts',(-9.19871798627596,-5.31086441980473,
-9.46010057379183));
#13734=CARTESIAN_POINT('Ctrl Pts',(-9.18229304117869,-5.30138994941625,
-9.4409200025508));
#13735=CARTESIAN_POINT('Ctrl Pts',(-9.16660604341306,-5.29234227360425,
-9.42086846723453));
#13736=CARTESIAN_POINT('Ctrl Pts',(-9.15175721629724,-5.28376928889603,
-9.39998581131754));
#13737=CARTESIAN_POINT('Ctrl Pts',(-9.13182856474318,-5.27226346263139,
-9.37195914159832));
#13738=CARTESIAN_POINT('Ctrl Pts',(-9.11351521748966,-5.26164700778255,
-9.34258220711578));
#13739=CARTESIAN_POINT('Ctrl Pts',(-9.09700209817711,-5.25207548543112,
-9.31197696571696));
#13740=CARTESIAN_POINT('Ctrl Pts',(-9.08187618167217,-5.24330802937557,
-9.28394275139018));
#13741=CARTESIAN_POINT('Ctrl Pts',(-9.06826135533797,-5.23541758926273,
-9.2548764399327));
#13742=CARTESIAN_POINT('Ctrl Pts',(-9.05633367221833,-5.2285208428221,-9.22490110097916));
#13743=CARTESIAN_POINT('Ctrl Pts',(-9.04538493587851,-5.22219013654632,
-9.1973859432065));
#13744=CARTESIAN_POINT('Ctrl Pts',(-9.03585874901313,-5.21669683169049,
-9.16910418723661));
#13745=CARTESIAN_POINT('Ctrl Pts',(-9.02790971986095,-5.2121260329523,-9.14019098056147));
#13746=CARTESIAN_POINT('Ctrl Pts',(-9.02027081268773,-5.20773355852555,
-9.11240578847789));
#13747=CARTESIAN_POINT('Ctrl Pts',(-9.01408944739803,-5.20419309163258,
-9.08403702004755));
#13748=CARTESIAN_POINT('Ctrl Pts',(-9.00950634701575,-5.20157374064314,
-9.0552511510112));
#13749=CARTESIAN_POINT('Ctrl Pts',(-9.0051246078554,-5.19906947238633,-9.02773000613096));
#13750=CARTESIAN_POINT('Ctrl Pts',(-9.002204824453,-5.19740715548407,-8.99982768780994));
#13751=CARTESIAN_POINT('Ctrl Pts',(-9.00085816830124,-5.1966406953204,-8.97173538759073));
#13752=CARTESIAN_POINT('Ctrl Pts',(-9.00028875667948,-5.19631661012298,
-8.95985701596189));
#13753=CARTESIAN_POINT('Ctrl Pts',(-9.00000036310671,-5.19615261240624,
-8.94794524541767));
#13754=CARTESIAN_POINT('Ctrl Pts',(-9.00000000034277,-5.19615242287113,
-8.93601699624085));
#13755=CARTESIAN_POINT('Ctrl Pts',(-2.90734818439019E-11,-10.3923048457926,
-8.93601699624128));
#13756=CARTESIAN_POINT('Ctrl Pts',(-4.10642892561727E-8,-10.3923058149047,
-8.96427557571348));
#13757=CARTESIAN_POINT('Ctrl Pts',(-1.27558244240631E-5,-10.3941683544014,
-8.9924385290414));
#13758=CARTESIAN_POINT('Ctrl Pts',(-3.18146852205633E-5,-10.3977787368057,
-9.02029415413065));
#13759=CARTESIAN_POINT('Ctrl Pts',(-5.15275647690907E-5,-10.4015130121237,
-9.04910566537449));
#13760=CARTESIAN_POINT('Ctrl Pts',(-7.7414908830901E-5,-10.4071161272311,
-9.07758819694581));
#13761=CARTESIAN_POINT('Ctrl Pts',(-9.83587654872778E-5,-10.4144403013317,
-9.10555931636106));
#13762=CARTESIAN_POINT('Ctrl Pts',(-0.000120807532366093,-10.4222907502563,
-9.13554028640848));
#13763=CARTESIAN_POINT('Ctrl Pts',(-0.000136929653821073,-10.4321173156833,
-9.16493372802667));
#13764=CARTESIAN_POINT('Ctrl Pts',(-0.000138635033354084,-10.4437307211343,
-9.1935757361048));
#13765=CARTESIAN_POINT('Ctrl Pts',(-0.000140425004800706,-10.4559201861495,
-9.22363847325004));
#13766=CARTESIAN_POINT('Ctrl Pts',(-0.000125857207500358,-10.4700770096022,
-9.252874295224));
#13767=CARTESIAN_POINT('Ctrl Pts',(-0.000100780446528402,-10.4859934580781,
-9.2811507783596));
#13768=CARTESIAN_POINT('Ctrl Pts',(-7.31620606961085E-5,-10.5035230989907,
-9.31229319033588));
#13769=CARTESIAN_POINT('Ctrl Pts',(-3.24759853636551E-5,-10.5231860217892,
-9.34227343310186));
#13770=CARTESIAN_POINT('Ctrl Pts',(-1.17901018813735E-5,-10.5447373137949,
-9.37096347131022));
#13771=CARTESIAN_POINT('Ctrl Pts',(-4.70298657794152E-6,-10.5521209235649,
-9.38079286095251));
#13772=CARTESIAN_POINT('Ctrl Pts',(-1.81298691785883E-7,-10.5597265189714,
-9.39047108282798));
#13773=CARTESIAN_POINT('Ctrl Pts',(-1.77170306928887E-7,-10.5675452688574,
-9.39999358405634));
#13774=CARTESIAN_POINT('Ctrl Pts',(-1.64365910958916E-7,-10.5917955199845,
-9.42952810677552));
#13775=CARTESIAN_POINT('Ctrl Pts',(-1.40786991299795E-5,-10.6179922639664,
-9.45742229073908));
#13776=CARTESIAN_POINT('Ctrl Pts',(-2.3249300100427E-5,-10.6458168703524,
-9.4835474262003));
#13777=CARTESIAN_POINT('Ctrl Pts',(-3.45972702524547E-5,-10.6802478529868,
-9.51587543375258));
#13778=CARTESIAN_POINT('Ctrl Pts',(-3.8706976771203E-5,-10.7171709180177,
-9.5454959152349));
#13779=CARTESIAN_POINT('Ctrl Pts',(-3.39070251259832E-5,-10.7560291195714,
-9.57222637923024));
#13780=CARTESIAN_POINT('Ctrl Pts',(-2.8201444964252E-5,-10.8022188731966,
-9.60400020037645));
#13781=CARTESIAN_POINT('Ctrl Pts',(-1.27781523534252E-5,-10.8511471894092,
-9.63169251308496));
#13782=CARTESIAN_POINT('Ctrl Pts',(-5.34813184271594E-6,-10.9019135377996,
-9.65503883152351));
#13783=CARTESIAN_POINT('Ctrl Pts',(-1.72253203311199E-6,-10.9266858063004,
-9.6664310487541));
#13784=CARTESIAN_POINT('Ctrl Pts',(5.95818053386175E-8,-10.9518957124607,
-9.67678873846151));
#13785=CARTESIAN_POINT('Ctrl Pts',(7.20244415219895E-8,-10.9774346496439,
-9.68608418837616));
#13786=CARTESIAN_POINT('Ctrl Pts',(-0.416515850482077,-10.6327803838108,
-9.02143340818646));
#13787=CARTESIAN_POINT('Ctrl Pts',(-0.333479226631307,-10.584839166678,
-9.54376732264983));
#13788=CARTESIAN_POINT('Ctrl Pts',(-0.0552692782898434,-11.0100828510945,
-9.69801774536257));
#13789=CARTESIAN_POINT('Ctrl Pts',(1.17171480220768,-9.7158149889452,-8.68478716585303));
#13790=CARTESIAN_POINT('Ctrl Pts',(1.21903459018144,-9.68849489662272,-9.20046647830121));
#13791=CARTESIAN_POINT('Ctrl Pts',(1.4992457995972,-10.0923950708269,-9.36117071967617));
#13792=CARTESIAN_POINT('Ctrl Pts',(2.79057777433264,-8.78116401620774,-8.46511979781123));
#13793=CARTESIAN_POINT('Ctrl Pts',(2.82267811638498,-8.76263087508485,-8.96938931321236));
#13794=CARTESIAN_POINT('Ctrl Pts',(3.07086796984993,-9.16662705077884,-9.14170490909608));
#13795=CARTESIAN_POINT('Ctrl Pts',(5.30300476213529,-7.33061361848059,-8.4607958473145));
#13796=CARTESIAN_POINT('Ctrl Pts',(5.28780275335659,-7.33939050234015,-8.9649080890023));
#13797=CARTESIAN_POINT('Ctrl Pts',(5.51949356046498,-7.75256486530674,-9.13738096491987));
#13798=CARTESIAN_POINT('Ctrl Pts',(6.13446031478957,-6.85057253133643,-8.51288388844));
#13799=CARTESIAN_POINT('Ctrl Pts',(6.1062759854001,-6.86684476149545,-9.01926238740732));
#13800=CARTESIAN_POINT('Ctrl Pts',(6.33184000468667,-7.28788066400649,-9.18946890902303));
#13801=CARTESIAN_POINT('Ctrl Pts',(7.78422102241503,-5.8980827426904,-8.70732652632487));
#13802=CARTESIAN_POINT('Ctrl Pts',(7.72763786808632,-5.93075104207461,-9.22034895088645));
#13803=CARTESIAN_POINT('Ctrl Pts',(7.95087159095549,-6.36753199333221,-9.38391126097247));
#13804=CARTESIAN_POINT('Ctrl Pts',(8.60317198574983,-5.42526118355596,-8.84899630416909));
#13805=CARTESIAN_POINT('Ctrl Pts',(8.53498342106806,-5.4646298697288,-9.36716113818546));
#13806=CARTESIAN_POINT('Ctrl Pts',(8.75804182449227,-5.91138165517438,-9.52557002452023));
#13807=CARTESIAN_POINT('Ctrl Pts',(9.41797736973474,-4.95483307577511,-9.02174323061993));
#13808=CARTESIAN_POINT('Ctrl Pts',(9.33492091061444,-5.00278574480615,-9.5440861505843));
#13809=CARTESIAN_POINT('Ctrl Pts',(9.56409180701241,-5.45636070606741,-9.69832756741748));
#13810=CARTESIAN_POINT('Ctrl Pts',(9.00000000031458,-5.19615242292188,-8.93601701648795));
#13811=CARTESIAN_POINT('Ctrl Pts',(9.00000081983887,-5.1961529434644,-8.96427559612485));
#13812=CARTESIAN_POINT('Ctrl Pts',(9.00160746974801,-5.19709522496851,-8.99243854955995));
#13813=CARTESIAN_POINT('Ctrl Pts',(9.00472462396319,-5.198916922074,-9.02029417470534));
#13814=CARTESIAN_POINT('Ctrl Pts',(9.00794874561115,-5.20080113205156,-9.04910568605485));
#13815=CARTESIAN_POINT('Ctrl Pts',(9.01278824276164,-5.20362510916489,-9.07758821767627));
#13816=CARTESIAN_POINT('Ctrl Pts',(9.01912069246065,-5.20730533458325,-9.10555933709354));
#13817=CARTESIAN_POINT('Ctrl Pts',(9.02590815713673,-5.21125000074161,-9.13554030717923));
#13818=CARTESIAN_POINT('Ctrl Pts',(9.03441015222614,-5.21617724611114,-9.16493374877919));
#13819=CARTESIAN_POINT('Ctrl Pts',(9.04446680453275,-5.22198542622267,-9.19357575679092));
#13820=CARTESIAN_POINT('Ctrl Pts',(9.05502229682808,-5.22808170941394,-9.22363849393975));
#13821=CARTESIAN_POINT('Ctrl Pts',(9.06728975039373,-5.23514750557975,-9.25287431586034));
#13822=CARTESIAN_POINT('Ctrl Pts',(9.0810863384078,-5.24308401322878,-9.28115079889175));
#13823=CARTESIAN_POINT('Ctrl Pts',(9.09628126293037,-5.25182491602132,-9.31229321069587));
#13824=CARTESIAN_POINT('Ctrl Pts',(9.11333019759206,-5.26162114280348,-9.34227345323255));
#13825=CARTESIAN_POINT('Ctrl Pts',(9.13200450784775,-5.27237887486722,-9.37096349115774));
#13826=CARTESIAN_POINT('Ctrl Pts',(9.13840244098876,-5.27606453980212,-9.38079287398074));
#13827=CARTESIAN_POINT('Ctrl Pts',(9.14499133635352,-5.27986341912618,-9.39047108923729));
#13828=CARTESIAN_POINT('Ctrl Pts',(9.1517625698874,-5.28377278786267,-9.39999358405638));
#13829=CARTESIAN_POINT('Ctrl Pts',(9.17276390981393,-5.29589790233735,-9.42952810677569));
#13830=CARTESIAN_POINT('Ctrl Pts',(9.19544399843216,-5.30900832449442,-9.45742229073938));
#13831=CARTESIAN_POINT('Ctrl Pts',(9.21953622911234,-5.32292856966092,-9.4835474262007));
#13832=CARTESIAN_POINT('Ctrl Pts',(9.24934866076502,-5.3401538886081,-9.51587543375205));
#13833=CARTESIAN_POINT('Ctrl Pts',(9.28132291821314,-5.35861898023332,-9.54549591523359));
#13834=CARTESIAN_POINT('Ctrl Pts',(9.31497750787883,-5.37804392412957,-9.57222637922831));
#13835=CARTESIAN_POINT('Ctrl Pts',(9.35498186070127,-5.40113385976393,-9.6040002003735));
#13836=CARTESIAN_POINT('Ctrl Pts',(9.39736273715034,-5.42558466090601,-9.63169251308128));
#13837=CARTESIAN_POINT('Ctrl Pts',(9.4413313995222,-5.45096140051353,-9.65503883151944));
#13838=CARTESIAN_POINT('Ctrl Pts',(9.46278662615571,-5.46334439490381,-9.66643104875163));
#13839=CARTESIAN_POINT('Ctrl Pts',(9.48461993637701,-5.47594780462949,-9.67678873846038));
#13840=CARTESIAN_POINT('Ctrl Pts',(9.50673731098735,-5.4887172624469,-9.68608418837614));
#13841=CARTESIAN_POINT('Ctrl Pts',(-9.,5.67710804811706,-9.02143424315509));
#13842=CARTESIAN_POINT('Ctrl Pts',(-9.,5.58122826343245,-9.54375341158405));
#13843=CARTESIAN_POINT('Ctrl Pts',(-9.50735826663105,5.55291153619582,-9.69801293012095));
#13844=CARTESIAN_POINT('Ctrl Pts',(-9.,3.84304933649568,-8.68476431765287));
#13845=CARTESIAN_POINT('Ctrl Pts',(-9.0000000000016,3.78841469353132,-9.20042897477229));
#13846=CARTESIAN_POINT('Ctrl Pts',(-9.48987412151624,3.74769245548026,-9.3611418811313));
#13847=CARTESIAN_POINT('Ctrl Pts',(-9.,1.97362405991046,-8.46509342346937));
#13848=CARTESIAN_POINT('Ctrl Pts',(-9.,1.93656169730459,-8.96934796476675));
#13849=CARTESIAN_POINT('Ctrl Pts',(-9.47394637335796,1.92362385779232,-9.14167211079771));
#13850=CARTESIAN_POINT('Ctrl Pts',(-9.,-0.927645358236382,-8.46080823523173));
#13851=CARTESIAN_POINT('Ctrl Pts',(-9.,-0.910084670211163,-8.96490692122887));
#13852=CARTESIAN_POINT('Ctrl Pts',(-9.47364809996973,-0.904144222134296,
-9.13738692201634));
#13853=CARTESIAN_POINT('Ctrl Pts',(-9.,-1.88752338654127,-8.5129006820434));
#13854=CARTESIAN_POINT('Ctrl Pts',(-9.,-1.85497578383212,-9.0192656693921));
#13855=CARTESIAN_POINT('Ctrl Pts',(-9.47739316073685,-1.83980071118508,
-9.18947936857881));
#13856=CARTESIAN_POINT('Ctrl Pts',(-9.,-3.7923825728723,-8.7073405558973));
#13857=CARTESIAN_POINT('Ctrl Pts',(-9.,-3.72704613553677,-9.22034905417095));
#13858=CARTESIAN_POINT('Ctrl Pts',(-9.48986299758601,-3.70198073363909,
-9.38391924329362));
#13859=CARTESIAN_POINT('Ctrl Pts',(-9.,-4.73797542141407,-8.84900381462939));
#13860=CARTESIAN_POINT('Ctrl Pts',(-9.00000000000247,-4.65923931810371,
-9.36715420610053));
#13861=CARTESIAN_POINT('Ctrl Pts',(-9.49840964046578,-4.62903686950057,
-9.52557170693384));
#13862=CARTESIAN_POINT('Ctrl Pts',(-9.,-5.67878800057612,-9.02174265850467));
#13863=CARTESIAN_POINT('Ctrl Pts',(-9.,-5.58288541678637,-9.54407079115471));
#13864=CARTESIAN_POINT('Ctrl Pts',(-9.5073742726743,-5.55456408813261,-9.69832134547053));
#13865=CARTESIAN_POINT('Ctrl Pts',(-9.50673731098736,5.48871726244691,-9.68608418837615));
#13866=CARTESIAN_POINT('Ctrl Pts',(-9.46751090700237,5.46606991294245,-9.66959818674222));
#13867=CARTESIAN_POINT('Ctrl Pts',(-9.4292555139926,5.44398741281737,-9.64980241574297));
#13868=CARTESIAN_POINT('Ctrl Pts',(-9.39244736393246,5.42274652050346,-9.62687224800763));
#13869=CARTESIAN_POINT('Ctrl Pts',(-9.35125753785235,5.39897709284228,-9.60121245202594));
#13870=CARTESIAN_POINT('Ctrl Pts',(-9.31187626544443,5.37625584557009,-9.57162847358945));
#13871=CARTESIAN_POINT('Ctrl Pts',(-9.27496301517173,5.35494322921267,-9.53835416024961));
#13872=CARTESIAN_POINT('Ctrl Pts',(-9.24815172482378,5.33946318502768,-9.51418594776514));
#13873=CARTESIAN_POINT('Ctrl Pts',(-9.22264230677134,5.324725264057,-9.48806927473095));
#13874=CARTESIAN_POINT('Ctrl Pts',(-9.19870255635967,5.31089128345573,-9.46010063975213));
#13875=CARTESIAN_POINT('Ctrl Pts',(-9.1822849306166,5.30140408696692,-9.44092004790256));
#13876=CARTESIAN_POINT('Ctrl Pts',(-9.16660589513319,5.29234257523934,-9.42086848991658));
#13877=CARTESIAN_POINT('Ctrl Pts',(-9.15175704158874,5.28376959610175,-9.39998580942839));
#13878=CARTESIAN_POINT('Ctrl Pts',(-9.13182837913581,5.27226379149956,-9.3719591412876));
#13879=CARTESIAN_POINT('Ctrl Pts',(-9.1134775869241,5.26171219558187,-9.34258220859915));
#13880=CARTESIAN_POINT('Ctrl Pts',(-9.09693184649301,5.25219717637988,-9.31197696915498));
#13881=CARTESIAN_POINT('Ctrl Pts',(-9.08177604900606,5.24348147672834,-9.28394275618111));
#13882=CARTESIAN_POINT('Ctrl Pts',(-9.06813531450727,5.23563591146739,-9.25487644617962));
#13883=CARTESIAN_POINT('Ctrl Pts',(-9.05619871536813,5.22875460811564,-9.22490110874421));
#13884=CARTESIAN_POINT('Ctrl Pts',(-9.04524179434031,5.22243807720807,-9.19738595126647));
#13885=CARTESIAN_POINT('Ctrl Pts',(-9.03572135889103,5.21693480952055,-9.16910419558254));
#13886=CARTESIAN_POINT('Ctrl Pts',(-9.02778841599091,5.21233614735411,-9.14019098916249));
#13887=CARTESIAN_POINT('Ctrl Pts',(-9.02016496747924,5.20791689655528,-9.11240579730802));
#13888=CARTESIAN_POINT('Ctrl Pts',(-9.01400815004361,5.20433391022739,-9.0840370290776));
#13889=CARTESIAN_POINT('Ctrl Pts',(-9.00944817481981,5.20167450390064,-9.05525116019153));
#13890=CARTESIAN_POINT('Ctrl Pts',(-9.00508854480459,5.19913194016382,-9.02773001548115));
#13891=CARTESIAN_POINT('Ctrl Pts',(-9.00218904391566,5.19743449151929,-8.99982769728534));
#13892=CARTESIAN_POINT('Ctrl Pts',(-9.00085194133044,5.1966514826345,-8.97173539712726));
#13893=CARTESIAN_POINT('Ctrl Pts',(-9.0002865694687,5.19632040019114,-8.95985702951628));
#13894=CARTESIAN_POINT('Ctrl Pts',(-9.00000034626581,5.19615264266129,-8.947945263001));
#13895=CARTESIAN_POINT('Ctrl Pts',(-9.00000000031462,5.19615242292189,-8.93601701784535));
#13896=CARTESIAN_POINT('Ctrl Pts',(9.,-5.67710138297224,-9.02143301966492));
#13897=CARTESIAN_POINT('Ctrl Pts',(9.,-5.58121904513111,-9.54376655404368));
#13898=CARTESIAN_POINT('Ctrl Pts',(9.5073763234892,-5.55290396848635,-9.69801721577213));
#13899=CARTESIAN_POINT('Ctrl Pts',(9.,-3.84322958818909,-8.68479770034242));
#13900=CARTESIAN_POINT('Ctrl Pts',(9.,-3.78858774329166,-9.20047677759492));
#13901=CARTESIAN_POINT('Ctrl Pts',(9.48989350969518,-3.74786882415842,-9.3611811508237));
#13902=CARTESIAN_POINT('Ctrl Pts',(9.,-1.97401147132877,-8.46514012239073));
#13903=CARTESIAN_POINT('Ctrl Pts',(9.,-1.93694391502001,-8.96941003041365));
#13904=CARTESIAN_POINT('Ctrl Pts',(9.47396685145451,-1.92400102339044,-9.14172507325324));
#13905=CARTESIAN_POINT('Ctrl Pts',(9.,0.926883757386691,-8.46078630815419));
#13906=CARTESIAN_POINT('Ctrl Pts',(9.,0.909336207055026,-8.96489785481209));
#13907=CARTESIAN_POINT('Ctrl Pts',(9.47366379315207,0.903401719775828,-9.13737126521503));
#13908=CARTESIAN_POINT('Ctrl Pts',(9.,1.88715353767526,-8.51287122562915));
#13909=CARTESIAN_POINT('Ctrl Pts',(9.,1.85461215070573,-9.01924893473238));
#13910=CARTESIAN_POINT('Ctrl Pts',(9.47740850275143,1.83943906473165,-9.18945608808641));
#13911=CARTESIAN_POINT('Ctrl Pts',(9.,3.79222649301937,-8.70731633004835));
#13912=CARTESIAN_POINT('Ctrl Pts',(9.,3.72689115576847,-9.22033807316646));
#13913=CARTESIAN_POINT('Ctrl Pts',(9.48987919364789,3.70182678106926,-9.383900913727));
#13914=CARTESIAN_POINT('Ctrl Pts',(9.,4.73790659517861,-8.84899105760459));
#13915=CARTESIAN_POINT('Ctrl Pts',(9.,4.65916993880134,-9.36715542952161));
#13916=CARTESIAN_POINT('Ctrl Pts',(9.49842686847536,4.62896805034413,-9.52556463079721));
#13917=CARTESIAN_POINT('Ctrl Pts',(9.,5.67879329673354,-9.02174363091134));
#13918=CARTESIAN_POINT('Ctrl Pts',(9.,5.58288799679954,-9.54408619370965));
#13919=CARTESIAN_POINT('Ctrl Pts',(9.50739244391453,5.55456828647369,-9.6983278266485));
#13920=CARTESIAN_POINT('Ctrl Pts',(9.0000000003434,5.19615242287113,-8.9360169962408));
#13921=CARTESIAN_POINT('Ctrl Pts',(9.00000086053094,5.19615287188961,-8.96427557554858));
#13922=CARTESIAN_POINT('Ctrl Pts',(9.00162022478813,5.19707313031505,-8.99243852866675));
#13923=CARTESIAN_POINT('Ctrl Pts',(9.00475643740047,5.19886181605305,-9.0202941535193));
#13924=CARTESIAN_POINT('Ctrl Pts',(9.00800027144488,5.20071188185179,-9.04910566453395));
#13925=CARTESIAN_POINT('Ctrl Pts',(9.01286565539748,5.2034910203135,-9.07758819584685));
#13926=CARTESIAN_POINT('Ctrl Pts',(9.01921904834677,5.20713496946256,-9.10555931499254));
#13927=CARTESIAN_POINT('Ctrl Pts',(9.02602896110547,5.21104075271889,-9.13554028463599));
#13928=CARTESIAN_POINT('Ctrl Pts',(9.03454707754073,5.21594007325843,-9.16493372584192));
#13929=CARTESIAN_POINT('Ctrl Pts',(9.0446054343648,5.22174529904746,-9.19357573352205));
#13930=CARTESIAN_POINT('Ctrl Pts',(9.05516271560771,5.2278384813043,-9.22363846998386));
#13931=CARTESIAN_POINT('Ctrl Pts',(9.06741560021868,5.23492950897316,-9.25287429130466));
#13932=CARTESIAN_POINT('Ctrl Pts',(9.08118711020269,5.24290945012497,-9.28115077384541));
#13933=CARTESIAN_POINT('Ctrl Pts',(9.09635441441848,5.25169818826729,-9.31229318403473));
#13934=CARTESIAN_POINT('Ctrl Pts',(9.11336266082172,5.26156488415088,-9.34227342516874));
#13935=CARTESIAN_POINT('Ctrl Pts',(9.13201628280739,5.27235844388821,-9.37096346195156));
#13936=CARTESIAN_POINT('Ctrl Pts',(9.13840713436601,5.27605638727547,-9.38079285414313));
#13937=CARTESIAN_POINT('Ctrl Pts',(9.1449915139327,5.27986310181482,-9.39047107849866));
#13938=CARTESIAN_POINT('Ctrl Pts',(9.15176274956368,5.2837724813323,-9.39999358213585));
#13939=CARTESIAN_POINT('Ctrl Pts',(9.17276407693867,5.2958976182429,-9.42952810540652));
#13940=CARTESIAN_POINT('Ctrl Pts',(9.19545808017158,5.30898394063489,-9.45742228997671));
#13941=CARTESIAN_POINT('Ctrl Pts',(9.21955948177444,5.32288830241885,-9.48354742602077));
#13942=CARTESIAN_POINT('Ctrl Pts',(9.24938325823851,5.3400939647514,-9.51587543043768));
#13943=CARTESIAN_POINT('Ctrl Pts',(9.28136162178356,5.35855193648451,-9.5454959093921));
#13944=CARTESIAN_POINT('Ctrl Pts',(9.31501140762171,5.37798519202097,-9.57222637143016));
#13945=CARTESIAN_POINT('Ctrl Pts',(9.35501003305752,5.40108499755732,-9.60400017658687));
#13946=CARTESIAN_POINT('Ctrl Pts',(9.39737546199132,5.4255624983292,-9.63169247761706));
#13947=CARTESIAN_POINT('Ctrl Pts',(9.44133666898288,5.45095209217556,-9.65503878908946));
#13948=CARTESIAN_POINT('Ctrl Pts',(9.46278829527576,5.46334138073684,-9.66643102290868));
#13949=CARTESIAN_POINT('Ctrl Pts',(9.48461984970672,5.47594789224658,-9.6767887266977));
#13950=CARTESIAN_POINT('Ctrl Pts',(9.50673723892373,5.48871738724752,-9.68608418809832));
#13951=CARTESIAN_POINT('Ctrl Pts',(0.416515850482078,10.6327803838108,-9.02143340818645));
#13952=CARTESIAN_POINT('Ctrl Pts',(0.333479226631358,10.584839166678,-9.54376732264953));
#13953=CARTESIAN_POINT('Ctrl Pts',(0.0552692782900587,11.0100828510942,
-9.69801774536245));
#13954=CARTESIAN_POINT('Ctrl Pts',(-1.17171480220777,9.71581498894514,-8.68478716585237));
#13955=CARTESIAN_POINT('Ctrl Pts',(-1.21903459018308,9.68849489662884,-9.20046647829118));
#13956=CARTESIAN_POINT('Ctrl Pts',(-1.49924579959968,10.0923950708306,-9.36117071967749));
#13957=CARTESIAN_POINT('Ctrl Pts',(-2.79057777433264,8.78116401620773,-8.46511979781291));
#13958=CARTESIAN_POINT('Ctrl Pts',(-2.82267811638496,8.76263087508485,-8.96938931321375));
#13959=CARTESIAN_POINT('Ctrl Pts',(-3.07086796985,9.16662705077899,-9.14170490909614));
#13960=CARTESIAN_POINT('Ctrl Pts',(-5.30300476213529,7.33061361848059,-8.46079584731366));
#13961=CARTESIAN_POINT('Ctrl Pts',(-5.28780275335659,7.33939050234014,-8.96490808900116));
#13962=CARTESIAN_POINT('Ctrl Pts',(-5.51949356046466,7.75256486530618,-9.13738096491964));
#13963=CARTESIAN_POINT('Ctrl Pts',(-6.13446031478939,6.85057253133653,-8.51288388844));
#13964=CARTESIAN_POINT('Ctrl Pts',(-6.10627598540037,6.86684476149594,-9.01926238740701));
#13965=CARTESIAN_POINT('Ctrl Pts',(-6.33184000468647,7.28788066400655,-9.18946890902299));
#13966=CARTESIAN_POINT('Ctrl Pts',(-7.78422102241521,5.8980827426903,-8.70732652632487));
#13967=CARTESIAN_POINT('Ctrl Pts',(-7.72763786808578,5.93075104207426,-9.22034895088613));
#13968=CARTESIAN_POINT('Ctrl Pts',(-7.95087159095534,6.36753199333147,-9.38391126097224));
#13969=CARTESIAN_POINT('Ctrl Pts',(-8.60317198574941,5.42526118355619,-8.84899630417094));
#13970=CARTESIAN_POINT('Ctrl Pts',(-8.53498342106766,5.4646298697288,-9.36716113818699));
#13971=CARTESIAN_POINT('Ctrl Pts',(-8.75804182449212,5.91138165517439,-9.52557002452018));
#13972=CARTESIAN_POINT('Ctrl Pts',(-9.41797736973474,4.95483307577511,-9.02174323061993));
#13973=CARTESIAN_POINT('Ctrl Pts',(-9.33492091061449,5.00278574480612,-9.54408615058399));
#13974=CARTESIAN_POINT('Ctrl Pts',(-9.56409180701224,5.45636070606705,-9.69832756741736));
#13975=CARTESIAN_POINT('Ctrl Pts',(-7.20244197616182E-8,10.977434649644,
-9.68608418837618));
#13976=CARTESIAN_POINT('Ctrl Pts',(-5.00286340846749E-8,10.9321399125021,
-9.66959818672784));
#13977=CARTESIAN_POINT('Ctrl Pts',(3.64038997071435E-6,10.8879685202237,
-9.64980241570864));
#13978=CARTESIAN_POINT('Ctrl Pts',(1.25630774211914E-5,10.8454712810141,
-9.62687224794793));
#13979=CARTESIAN_POINT('Ctrl Pts',(2.25479297814334E-5,10.7979151314145,
-9.60121245195519));
#13980=CARTESIAN_POINT('Ctrl Pts',(3.60067895874637E-5,10.7524493254351,
-9.57162847350616));
#13981=CARTESIAN_POINT('Ctrl Pts',(3.53647383512323E-5,10.7098252047811,
-9.5383541601524));
#13982=CARTESIAN_POINT('Ctrl Pts',(3.48983957240436E-5,10.6788659241417,
-9.51418594766149));
#13983=CARTESIAN_POINT('Ctrl Pts',(2.61934615827083E-5,10.6494051595904,
-9.48806927462073));
#13984=CARTESIAN_POINT('Ctrl Pts',(1.54900307618859E-5,10.6217557372769,
-9.46010063963534));
#13985=CARTESIAN_POINT('Ctrl Pts',(8.14973197026581E-6,10.6027940581112,
-9.44092004782107));
#13986=CARTESIAN_POINT('Ctrl Pts',(1.68120725248121E-7,10.5846848592506,
-9.42086848987401));
#13987=CARTESIAN_POINT('Ctrl Pts',(1.77173693458057E-7,10.5675388853301,
-9.39998580942819));
#13988=CARTESIAN_POINT('Ctrl Pts',(1.89323691907141E-7,10.5445272551391,
-9.37195914135774));
#13989=CARTESIAN_POINT('Ctrl Pts',(3.76353141956738E-5,10.5233592049939,
-9.34258220874644));
#13990=CARTESIAN_POINT('Ctrl Pts',(7.02571832642839E-5,10.5042726638926,
-9.31197696938525));
#13991=CARTESIAN_POINT('Ctrl Pts',(0.000100138618398514,10.486789507466,
-9.28394275488897));
#13992=CARTESIAN_POINT('Ctrl Pts',(0.000126047045856005,10.4710535014604,
-9.25487644325188));
#13993=CARTESIAN_POINT('Ctrl Pts',(0.000134963100562419,10.4572754511472,
-9.22490110408888));
#13994=CARTESIAN_POINT('Ctrl Pts',(0.000143147383229936,10.4446282139908,
-9.19738594667423));
#13995=CARTESIAN_POINT('Ctrl Pts',(0.000137395485180129,10.4336316414396,
-9.16910419106805));
#13996=CARTESIAN_POINT('Ctrl Pts',(0.000121308674796911,10.4244621805141,
-9.14019098474074));
#13997=CARTESIAN_POINT('Ctrl Pts',(0.000105849472287728,10.4156504552578,
-9.11240579294972));
#13998=CARTESIAN_POINT('Ctrl Pts',(8.13010084074135E-5,10.408527002,-9.08403702479553));
#13999=CARTESIAN_POINT('Ctrl Pts',(5.81751825992234E-5,10.403248244655,
-9.0552511559988));
#14000=CARTESIAN_POINT('Ctrl Pts',(3.60654036386653E-5,10.3982014126389,
-9.02773001138921));
#14001=CARTESIAN_POINT('Ctrl Pts',(1.57822010900823E-5,10.3948416470749,
-8.9998276933066));
#14002=CARTESIAN_POINT('Ctrl Pts',(6.22790905404415E-6,10.3932921779994,
-8.9717353932735));
#14003=CARTESIAN_POINT('Ctrl Pts',(2.18803160560752E-6,10.3926370101281,
-8.95985701976865));
#14004=CARTESIAN_POINT('Ctrl Pts',(1.73508680193248E-8,10.3923052548651,
-8.94794524732802));
#14005=CARTESIAN_POINT('Ctrl Pts',(2.91081211519974E-11,10.3923048457926,
-8.93601699624122));
#14006=CARTESIAN_POINT('Ctrl Pts',(9.41651585048208,4.95567688430906,-9.02143340818645));
#14007=CARTESIAN_POINT('Ctrl Pts',(9.33347922663135,5.00361810144187,-9.54376732264957));
#14008=CARTESIAN_POINT('Ctrl Pts',(9.56264608596402,5.45717682649912,-9.69801774536247));
#14009=CARTESIAN_POINT('Ctrl Pts',(7.82828519779331,5.87264227917413,-8.68478716584893));
#14010=CARTESIAN_POINT('Ctrl Pts',(7.78096540982123,5.89996237149757,-9.20046647828723));
#14011=CARTESIAN_POINT('Ctrl Pts',(7.99064761656545,6.34458248438075,-9.3611707196757));
#14012=CARTESIAN_POINT('Ctrl Pts',(6.20942222566664,6.80729325191259,-8.46511979781291));
#14013=CARTESIAN_POINT('Ctrl Pts',(6.17732188361544,6.82582639303698,-8.96938931321379));
#14014=CARTESIAN_POINT('Ctrl Pts',(6.40309790806782,7.24276319894767,-9.14170490909629));
#14015=CARTESIAN_POINT('Ctrl Pts',(3.69699523786507,8.2578436496391,-8.46079584731366));
#14016=CARTESIAN_POINT('Ctrl Pts',(3.71219724664288,8.24906676577899,-8.96490808900122));
#14017=CARTESIAN_POINT('Ctrl Pts',(3.95417133760926,8.65630407204012,-9.13738096491959));
#14018=CARTESIAN_POINT('Ctrl Pts',(2.86553968521059,8.73788473678338,-8.51288388844));
#14019=CARTESIAN_POINT('Ctrl Pts',(2.89372401460009,8.72161250662446,-9.01926238740707));
#14020=CARTESIAN_POINT('Ctrl Pts',(3.14556979243603,9.12747462876021,-9.18946890902297));
#14021=CARTESIAN_POINT('Ctrl Pts',(1.21577897758481,9.69037452542958,-8.70732652632487));
#14022=CARTESIAN_POINT('Ctrl Pts',(1.27236213191344,9.65770622604531,-9.2203489508862));
#14023=CARTESIAN_POINT('Ctrl Pts',(1.53900867015742,10.0694227766613,-9.38391126097231));
#14024=CARTESIAN_POINT('Ctrl Pts',(0.396828014250648,10.1631960845637,-8.84899630417139));
#14025=CARTESIAN_POINT('Ctrl Pts',(0.465016578932603,10.1238273983911,-9.36716113818768));
#14026=CARTESIAN_POINT('Ctrl Pts',(0.740385772601153,10.540377535005,-9.52557002452055));
#14027=CARTESIAN_POINT('Ctrl Pts',(-0.417977369734738,10.6336241923448,
-9.02174323061993));
#14028=CARTESIAN_POINT('Ctrl Pts',(-0.334920910614486,10.5856715233138,
-9.54408615058404));
#14029=CARTESIAN_POINT('Ctrl Pts',(-0.0566989198408205,11.0109268220328,
-9.69832756741738));
#14030=CARTESIAN_POINT('',(0.,0.,0.));
#14031=CARTESIAN_POINT('Origin',(32.,329.539392014169,-8.2));
#14032=CARTESIAN_POINT('',(29.,329.539392014169,-6.2));
#14033=CARTESIAN_POINT('Origin',(32.,329.539392014169,-6.2));
#14034=CARTESIAN_POINT('',(29.,329.539392014169,-8.2));
#14035=CARTESIAN_POINT('',(29.,329.539392014169,-8.2));
#14036=CARTESIAN_POINT('Origin',(32.,329.539392014169,-8.2));
#14037=CARTESIAN_POINT('Origin',(32.,329.539392014169,8.2));
#14038=CARTESIAN_POINT('',(35.,329.539392014169,6.2));
#14039=CARTESIAN_POINT('Origin',(32.,329.539392014169,6.2));
#14040=CARTESIAN_POINT('',(35.,329.539392014169,8.2));
#14041=CARTESIAN_POINT('',(35.,329.539392014169,8.2));
#14042=CARTESIAN_POINT('Origin',(32.,329.539392014169,8.2));
#14043=CARTESIAN_POINT('Origin',(32.,329.539392014169,-11.5740115370178));
#14044=CARTESIAN_POINT('',(30.1,329.539392014169,6.2));
#14045=CARTESIAN_POINT('Origin',(32.,329.539392014169,6.2));
#14046=CARTESIAN_POINT('',(30.1,329.539392014169,-6.2));
#14047=CARTESIAN_POINT('',(30.1,329.539392014169,-11.5740115370178));
#14048=CARTESIAN_POINT('Origin',(32.,329.539392014169,-6.2));
#14049=CARTESIAN_POINT('Origin',(32.,329.539392014169,8.2));
#14050=CARTESIAN_POINT('Origin',(32.,329.539392014169,6.2));
#14051=CARTESIAN_POINT('Origin',(32.,329.539392014169,-8.2));
#14052=CARTESIAN_POINT('Origin',(32.,329.539392014169,-6.2));
#14053=CARTESIAN_POINT('',(0.,0.,0.));
#14054=CARTESIAN_POINT('',(0.,0.,0.));
#14055=CARTESIAN_POINT('',(0.,0.,0.));
#14056=CARTESIAN_POINT('',(0.,0.,0.));
#14057=CARTESIAN_POINT('',(0.,0.,0.));
#14058=CARTESIAN_POINT('',(0.,0.,0.));
#14059=CARTESIAN_POINT('',(0.,0.,0.));
#14060=CARTESIAN_POINT('',(0.,0.,0.));
#14061=CARTESIAN_POINT('',(0.,51.,0.));
#14062=CARTESIAN_POINT('',(-13.8464315415298,-6.58525409799449,0.));
#14063=UNCERTAINTY_MEASURE_WITH_UNIT(LENGTH_MEASURE(0.01),#14085,
'DISTANCE_ACCURACY_VALUE',
'Maximum model space distance between geometric entities at asserted c
onnectivities');
#14064=UNCERTAINTY_MEASURE_WITH_UNIT(LENGTH_MEASURE(0.01),#14085,
'DISTANCE_ACCURACY_VALUE',
'Maximum model space distance between geometric entities at asserted c
onnectivities');
#14065=UNCERTAINTY_MEASURE_WITH_UNIT(LENGTH_MEASURE(0.01),#14085,
'DISTANCE_ACCURACY_VALUE',
'Maximum model space distance between geometric entities at asserted c
onnectivities');
#14066=UNCERTAINTY_MEASURE_WITH_UNIT(LENGTH_MEASURE(0.01),#14085,
'DISTANCE_ACCURACY_VALUE',
'Maximum model space distance between geometric entities at asserted c
onnectivities');
#14067=UNCERTAINTY_MEASURE_WITH_UNIT(LENGTH_MEASURE(0.01),#14085,
'DISTANCE_ACCURACY_VALUE',
'Maximum model space distance between geometric entities at asserted c
onnectivities');
#14068=UNCERTAINTY_MEASURE_WITH_UNIT(LENGTH_MEASURE(0.01),#14085,
'DISTANCE_ACCURACY_VALUE',
'Maximum model space distance between geometric entities at asserted c
onnectivities');
#14069=UNCERTAINTY_MEASURE_WITH_UNIT(LENGTH_MEASURE(0.01),#14085,
'DISTANCE_ACCURACY_VALUE',
'Maximum model space distance between geometric entities at asserted c
onnectivities');
#14070=UNCERTAINTY_MEASURE_WITH_UNIT(LENGTH_MEASURE(0.01),#14085,
'DISTANCE_ACCURACY_VALUE',
'Maximum model space distance between geometric entities at asserted c
onnectivities');
#14071=UNCERTAINTY_MEASURE_WITH_UNIT(LENGTH_MEASURE(0.01),#14085,
'DISTANCE_ACCURACY_VALUE',
'Maximum model space distance between geometric entities at asserted c
onnectivities');
#14072=UNCERTAINTY_MEASURE_WITH_UNIT(LENGTH_MEASURE(0.01),#14085,
'DISTANCE_ACCURACY_VALUE',
'Maximum model space distance between geometric entities at asserted c
onnectivities');
#14073=UNCERTAINTY_MEASURE_WITH_UNIT(LENGTH_MEASURE(0.01),#14085,
'DISTANCE_ACCURACY_VALUE',
'Maximum model space distance between geometric entities at asserted c
onnectivities');
#14074=(
GEOMETRIC_REPRESENTATION_CONTEXT(3)
GLOBAL_UNCERTAINTY_ASSIGNED_CONTEXT((#14063))
GLOBAL_UNIT_ASSIGNED_CONTEXT((#14085,#14087,#14088))
REPRESENTATION_CONTEXT('','3D')
);
#14075=(
GEOMETRIC_REPRESENTATION_CONTEXT(3)
GLOBAL_UNCERTAINTY_ASSIGNED_CONTEXT((#14064))
GLOBAL_UNIT_ASSIGNED_CONTEXT((#14085,#14087,#14088))
REPRESENTATION_CONTEXT('','3D')
);
#14076=(
GEOMETRIC_REPRESENTATION_CONTEXT(3)
GLOBAL_UNCERTAINTY_ASSIGNED_CONTEXT((#14065))
GLOBAL_UNIT_ASSIGNED_CONTEXT((#14085,#14087,#14088))
REPRESENTATION_CONTEXT('','3D')
);
#14077=(
GEOMETRIC_REPRESENTATION_CONTEXT(3)
GLOBAL_UNCERTAINTY_ASSIGNED_CONTEXT((#14066))
GLOBAL_UNIT_ASSIGNED_CONTEXT((#14085,#14087,#14088))
REPRESENTATION_CONTEXT('','3D')
);
#14078=(
GEOMETRIC_REPRESENTATION_CONTEXT(3)
GLOBAL_UNCERTAINTY_ASSIGNED_CONTEXT((#14067))
GLOBAL_UNIT_ASSIGNED_CONTEXT((#14085,#14087,#14088))
REPRESENTATION_CONTEXT('','3D')
);
#14079=(
GEOMETRIC_REPRESENTATION_CONTEXT(3)
GLOBAL_UNCERTAINTY_ASSIGNED_CONTEXT((#14068))
GLOBAL_UNIT_ASSIGNED_CONTEXT((#14085,#14087,#14088))
REPRESENTATION_CONTEXT('','3D')
);
#14080=(
GEOMETRIC_REPRESENTATION_CONTEXT(3)
GLOBAL_UNCERTAINTY_ASSIGNED_CONTEXT((#14069))
GLOBAL_UNIT_ASSIGNED_CONTEXT((#14085,#14087,#14088))
REPRESENTATION_CONTEXT('','3D')
);
#14081=(
GEOMETRIC_REPRESENTATION_CONTEXT(3)
GLOBAL_UNCERTAINTY_ASSIGNED_CONTEXT((#14070))
GLOBAL_UNIT_ASSIGNED_CONTEXT((#14085,#14087,#14088))
REPRESENTATION_CONTEXT('','3D')
);
#14082=(
GEOMETRIC_REPRESENTATION_CONTEXT(3)
GLOBAL_UNCERTAINTY_ASSIGNED_CONTEXT((#14071))
GLOBAL_UNIT_ASSIGNED_CONTEXT((#14085,#14087,#14088))
REPRESENTATION_CONTEXT('','3D')
);
#14083=(
GEOMETRIC_REPRESENTATION_CONTEXT(3)
GLOBAL_UNCERTAINTY_ASSIGNED_CONTEXT((#14072))
GLOBAL_UNIT_ASSIGNED_CONTEXT((#14085,#14087,#14088))
REPRESENTATION_CONTEXT('','3D')
);
#14084=(
GEOMETRIC_REPRESENTATION_CONTEXT(3)
GLOBAL_UNCERTAINTY_ASSIGNED_CONTEXT((#14073))
GLOBAL_UNIT_ASSIGNED_CONTEXT((#14085,#14087,#14088))
REPRESENTATION_CONTEXT('','3D')
);
#14085=(
LENGTH_UNIT()
NAMED_UNIT(*)
SI_UNIT(.MILLI.,.METRE.)
);
#14086=(
LENGTH_UNIT()
NAMED_UNIT(*)
SI_UNIT($,.METRE.)
);
#14087=(
NAMED_UNIT(*)
PLANE_ANGLE_UNIT()
SI_UNIT($,.RADIAN.)
);
#14088=(
NAMED_UNIT(*)
SI_UNIT($,.STERADIAN.)
SOLID_ANGLE_UNIT()
);
#14089=SHAPE_DEFINITION_REPRESENTATION(#14099,#14119);
#14090=SHAPE_DEFINITION_REPRESENTATION(#14100,#14120);
#14091=SHAPE_DEFINITION_REPRESENTATION(#14101,#14121);
#14092=SHAPE_DEFINITION_REPRESENTATION(#14102,#14122);
#14093=SHAPE_DEFINITION_REPRESENTATION(#14103,#14123);
#14094=SHAPE_DEFINITION_REPRESENTATION(#14104,#14124);
#14095=SHAPE_DEFINITION_REPRESENTATION(#14105,#14125);
#14096=SHAPE_DEFINITION_REPRESENTATION(#14106,#14126);
#14097=SHAPE_DEFINITION_REPRESENTATION(#14107,#14127);
#14098=SHAPE_DEFINITION_REPRESENTATION(#14108,#14128);
#14099=PRODUCT_DEFINITION_SHAPE('',$,#14130);
#14100=PRODUCT_DEFINITION_SHAPE('',$,#14131);
#14101=PRODUCT_DEFINITION_SHAPE('',$,#14132);
#14102=PRODUCT_DEFINITION_SHAPE('',$,#14133);
#14103=PRODUCT_DEFINITION_SHAPE('',$,#14134);
#14104=PRODUCT_DEFINITION_SHAPE('',$,#14135);
#14105=PRODUCT_DEFINITION_SHAPE('',$,#14136);
#14106=PRODUCT_DEFINITION_SHAPE('',$,#14137);
#14107=PRODUCT_DEFINITION_SHAPE('',$,#14138);
#14108=PRODUCT_DEFINITION_SHAPE('',$,#14139);
#14109=PRODUCT_DEFINITION_SHAPE($,$,#41);
#14110=PRODUCT_DEFINITION_SHAPE($,$,#42);
#14111=PRODUCT_DEFINITION_SHAPE($,$,#43);
#14112=PRODUCT_DEFINITION_SHAPE($,$,#44);
#14113=PRODUCT_DEFINITION_SHAPE($,$,#45);
#14114=PRODUCT_DEFINITION_SHAPE($,$,#46);
#14115=PRODUCT_DEFINITION_SHAPE($,$,#47);
#14116=PRODUCT_DEFINITION_SHAPE($,$,#48);
#14117=PRODUCT_DEFINITION_SHAPE($,$,#49);
#14118=PRODUCT_DEFINITION_SHAPE($,$,#50);
#14119=SHAPE_REPRESENTATION('',(#3574,#3854,#3855,#3856,#3857,#3858,#3859,
#3860,#3861,#3862,#3863),#14074);
#14120=SHAPE_REPRESENTATION('',(#3575),#14075);
#14121=SHAPE_REPRESENTATION('',(#3597),#14076);
#14122=SHAPE_REPRESENTATION('',(#3649),#14077);
#14123=SHAPE_REPRESENTATION('',(#3725),#14078);
#14124=SHAPE_REPRESENTATION('',(#3741),#14079);
#14125=SHAPE_REPRESENTATION('',(#3763),#14080);
#14126=SHAPE_REPRESENTATION('',(#3794),#14081);
#14127=SHAPE_REPRESENTATION('',(#3802),#14082);
#14128=SHAPE_REPRESENTATION('',(#3840),#14083);
#14129=PRODUCT_DEFINITION_CONTEXT('part definition',#14161,'design');
#14130=PRODUCT_DEFINITION('Caulk Applicator Gun','TAS-005',#14140,#14129);
#14131=PRODUCT_DEFINITION('Cartridge holder','Cartridge holder',#14141,
#14129);
#14132=PRODUCT_DEFINITION('head','head',#14142,#14129);
#14133=PRODUCT_DEFINITION('centre rod','centre rod',#14143,#14129);
#14134=PRODUCT_DEFINITION('plunger','plunger',#14144,#14129);
#14135=PRODUCT_DEFINITION('catch plate','catch plate',#14145,#14129);
#14136=PRODUCT_DEFINITION('trigger','trigger',#14146,#14129);
#14137=PRODUCT_DEFINITION('spring','spring',#14147,#14129);
#14138=PRODUCT_DEFINITION(
'hex flange nut gradea_iso_ISO - 4161 - M12 - N',
'hex flange nut gradea_iso_ISO - 4161 - M12 - N',#14148,#14129);
#14139=PRODUCT_DEFINITION('rivet','rivet',#14149,#14129);
#14140=PRODUCT_DEFINITION_FORMATION('',$,#14163);
#14141=PRODUCT_DEFINITION_FORMATION('',$,#14164);
#14142=PRODUCT_DEFINITION_FORMATION('',$,#14165);
#14143=PRODUCT_DEFINITION_FORMATION('',$,#14166);
#14144=PRODUCT_DEFINITION_FORMATION('',$,#14167);
#14145=PRODUCT_DEFINITION_FORMATION('',$,#14168);
#14146=PRODUCT_DEFINITION_FORMATION('',$,#14169);
#14147=PRODUCT_DEFINITION_FORMATION('',$,#14170);
#14148=PRODUCT_DEFINITION_FORMATION('',$,#14171);
#14149=PRODUCT_DEFINITION_FORMATION('',$,#14172);
#14150=PRODUCT_RELATED_PRODUCT_CATEGORY('TAS-005','TAS-005',(#14163));
#14151=PRODUCT_RELATED_PRODUCT_CATEGORY('Cartridge holder',
'Cartridge holder',(#14164));
#14152=PRODUCT_RELATED_PRODUCT_CATEGORY('head','head',(#14165));
#14153=PRODUCT_RELATED_PRODUCT_CATEGORY('centre rod','centre rod',(#14166));
#14154=PRODUCT_RELATED_PRODUCT_CATEGORY('plunger','plunger',(#14167));
#14155=PRODUCT_RELATED_PRODUCT_CATEGORY('catch plate','catch plate',(#14168));
#14156=PRODUCT_RELATED_PRODUCT_CATEGORY('trigger','trigger',(#14169));
#14157=PRODUCT_RELATED_PRODUCT_CATEGORY('spring','spring',(#14170));
#14158=PRODUCT_RELATED_PRODUCT_CATEGORY(
'hex flange nut gradea_iso_ISO - 4161 - M12 - N',
'hex flange nut gradea_iso_ISO - 4161 - M12 - N',(#14171));
#14159=PRODUCT_RELATED_PRODUCT_CATEGORY('rivet','rivet',(#14172));
#14160=APPLICATION_PROTOCOL_DEFINITION('international standard',
'automotive_design',2009,#14161);
#14161=APPLICATION_CONTEXT(
'Core Data for Automotive Mechanical Design Process');
#14162=PRODUCT_CONTEXT('part definition',#14161,'mechanical');
#14163=PRODUCT('Caulk Applicator Gun','TAS-005','STEP AP214',(#14162));
#14164=PRODUCT('Cartridge holder','Cartridge holder',$,(#14162));
#14165=PRODUCT('head','head',$,(#14162));
#14166=PRODUCT('centre rod','centre rod',$,(#14162));
#14167=PRODUCT('plunger','plunger',$,(#14162));
#14168=PRODUCT('catch plate','catch plate',$,(#14162));
#14169=PRODUCT('trigger','trigger',$,(#14162));
#14170=PRODUCT('spring','spring',$,(#14162));
#14171=PRODUCT('hex flange nut gradea_iso_ISO - 4161 - M12 - N',
'hex flange nut gradea_iso_ISO - 4161 - M12 - N',$,(#14162));
#14172=PRODUCT('rivet','rivet',$,(#14162));
#14173=PRESENTATION_STYLE_ASSIGNMENT((#14179));
#14174=PRESENTATION_STYLE_ASSIGNMENT((#14180));
#14175=PRESENTATION_STYLE_ASSIGNMENT((#14181));
#14176=PRESENTATION_STYLE_ASSIGNMENT((#14182));
#14177=PRESENTATION_STYLE_ASSIGNMENT((#14183));
#14178=PRESENTATION_STYLE_ASSIGNMENT((#14184));
#14179=SURFACE_STYLE_USAGE(.BOTH.,#14185);
#14180=SURFACE_STYLE_USAGE(.BOTH.,#14186);
#14181=SURFACE_STYLE_USAGE(.BOTH.,#14187);
#14182=SURFACE_STYLE_USAGE(.BOTH.,#14188);
#14183=SURFACE_STYLE_USAGE(.BOTH.,#14189);
#14184=SURFACE_STYLE_USAGE(.BOTH.,#14190);
#14185=SURFACE_SIDE_STYLE('',(#14191));
#14186=SURFACE_SIDE_STYLE('',(#14192));
#14187=SURFACE_SIDE_STYLE('',(#14193));
#14188=SURFACE_SIDE_STYLE('',(#14194));
#14189=SURFACE_SIDE_STYLE('',(#14195));
#14190=SURFACE_SIDE_STYLE('',(#14196));
#14191=SURFACE_STYLE_FILL_AREA(#14197);
#14192=SURFACE_STYLE_FILL_AREA(#14198);
#14193=SURFACE_STYLE_FILL_AREA(#14199);
#14194=SURFACE_STYLE_FILL_AREA(#14200);
#14195=SURFACE_STYLE_FILL_AREA(#14201);
#14196=SURFACE_STYLE_FILL_AREA(#14202);
#14197=FILL_AREA_STYLE('Steel - Satin',(#14203));
#14198=FILL_AREA_STYLE('Opaque(97,158,199)',(#14204));
#14199=FILL_AREA_STYLE('Opaque(227,224,212)',(#14205));
#14200=FILL_AREA_STYLE('Opaque(122,133,145)',(#14206));
#14201=FILL_AREA_STYLE('Opaque(31,36,43)',(#14207));
#14202=FILL_AREA_STYLE('Opaque(61,176,222)',(#14208));
#14203=FILL_AREA_STYLE_COLOUR('Steel - Satin',#14209);
#14204=FILL_AREA_STYLE_COLOUR('Opaque(97,158,199)',#14210);
#14205=FILL_AREA_STYLE_COLOUR('Opaque(227,224,212)',#14211);
#14206=FILL_AREA_STYLE_COLOUR('Opaque(122,133,145)',#14212);
#14207=FILL_AREA_STYLE_COLOUR('Opaque(31,36,43)',#14213);
#14208=FILL_AREA_STYLE_COLOUR('Opaque(61,176,222)',#14214);
#14209=COLOUR_RGB('Steel - Satin',0.627450980392157,0.627450980392157,0.627450980392157);
#14210=COLOUR_RGB('Opaque(97,158,199)',0.380392156862745,0.619607843137255,
0.780392156862745);
#14211=COLOUR_RGB('Opaque(227,224,212)',0.890196078431372,0.87843137254902,
0.831372549019608);
#14212=COLOUR_RGB('Opaque(122,133,145)',0.47843137254902,0.52156862745098,
0.568627450980392);
#14213=COLOUR_RGB('Opaque(31,36,43)',0.12156862745098,0.141176470588235,
0.168627450980392);
#14214=COLOUR_RGB('Opaque(61,176,222)',0.23921568627451,0.690196078431373,
0.870588235294118);
ENDSEC;
END-ISO-10303-21;
